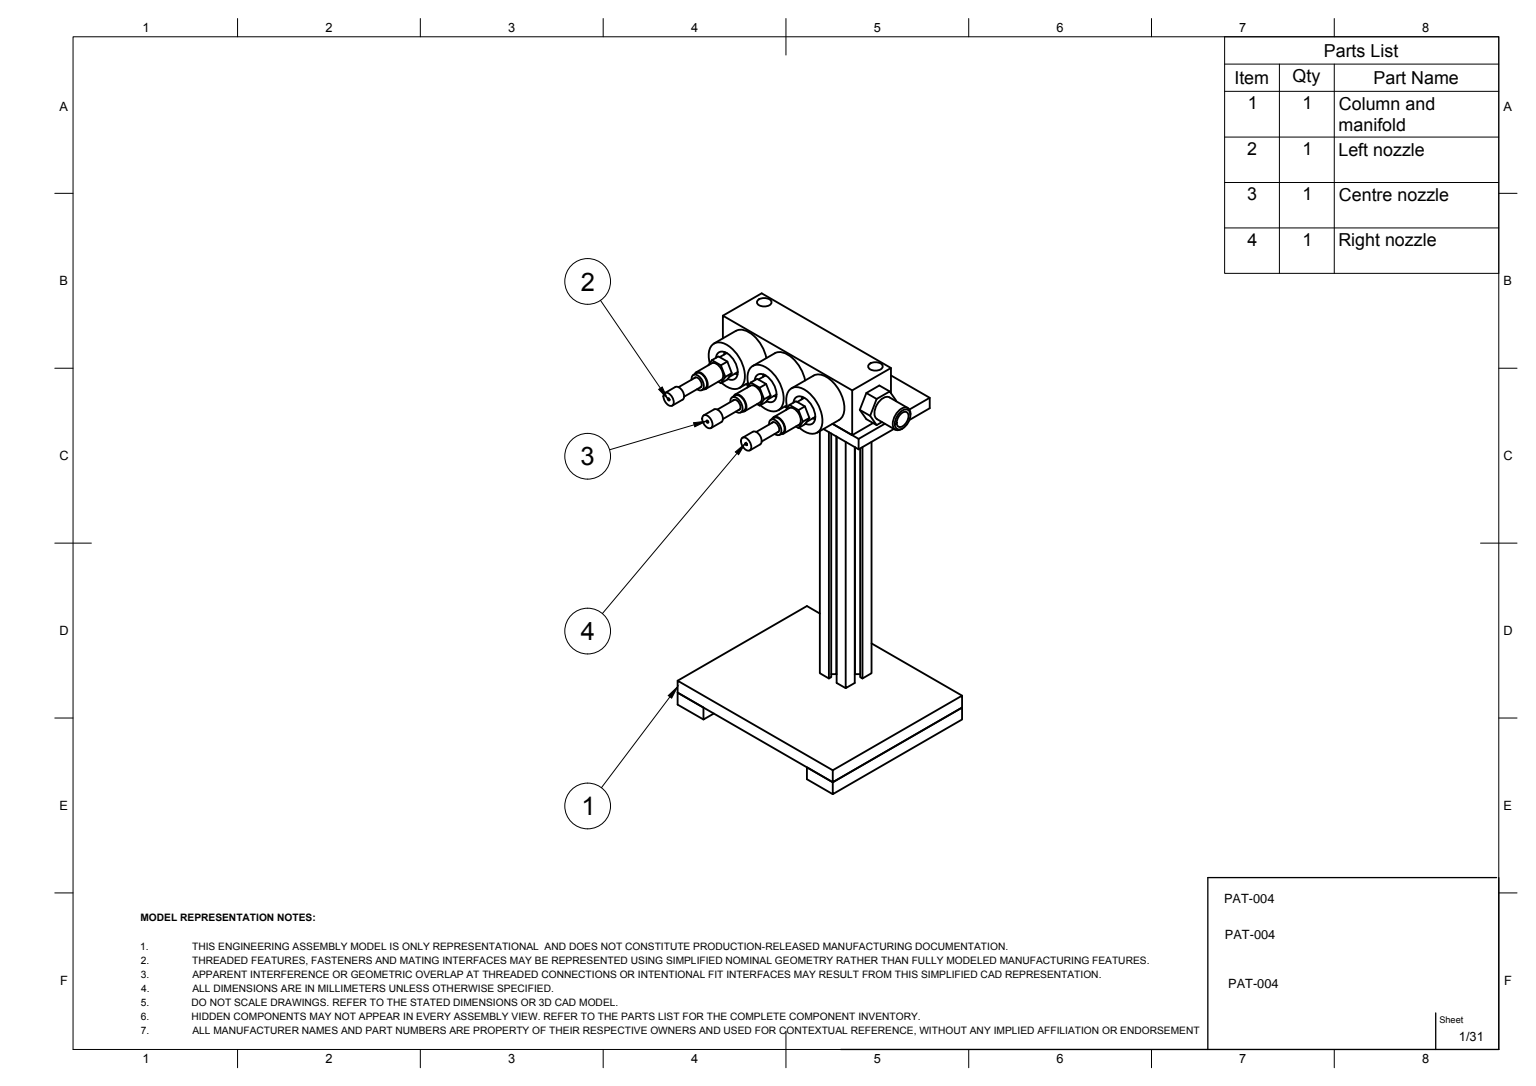
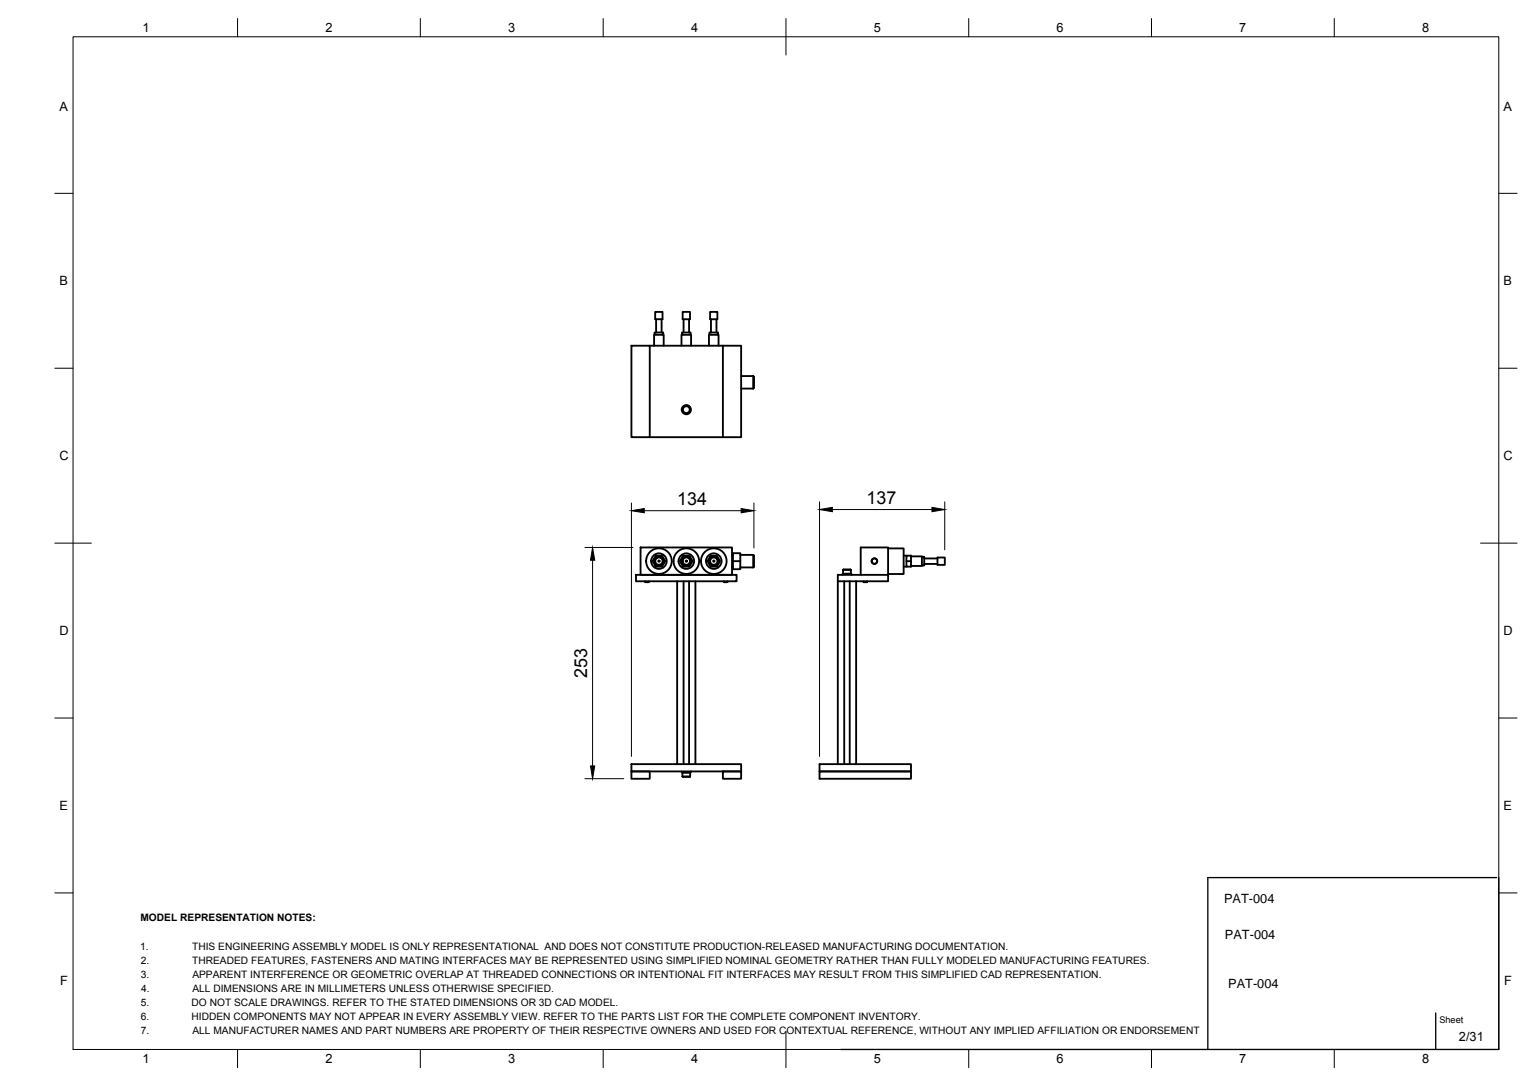
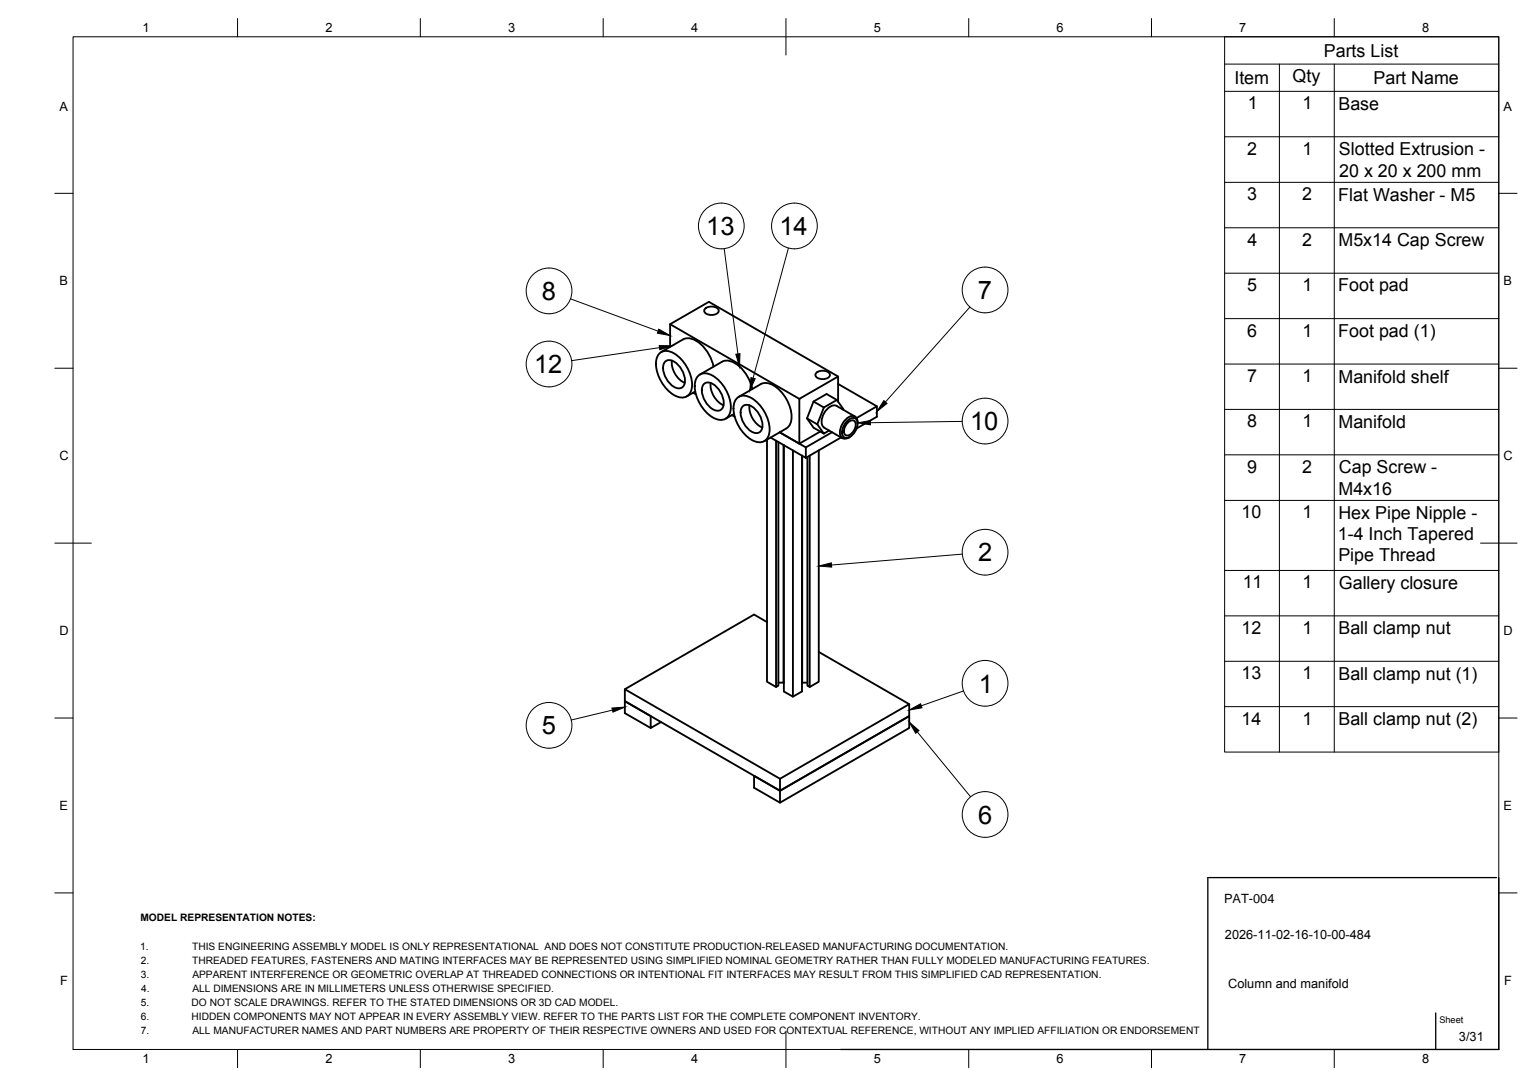
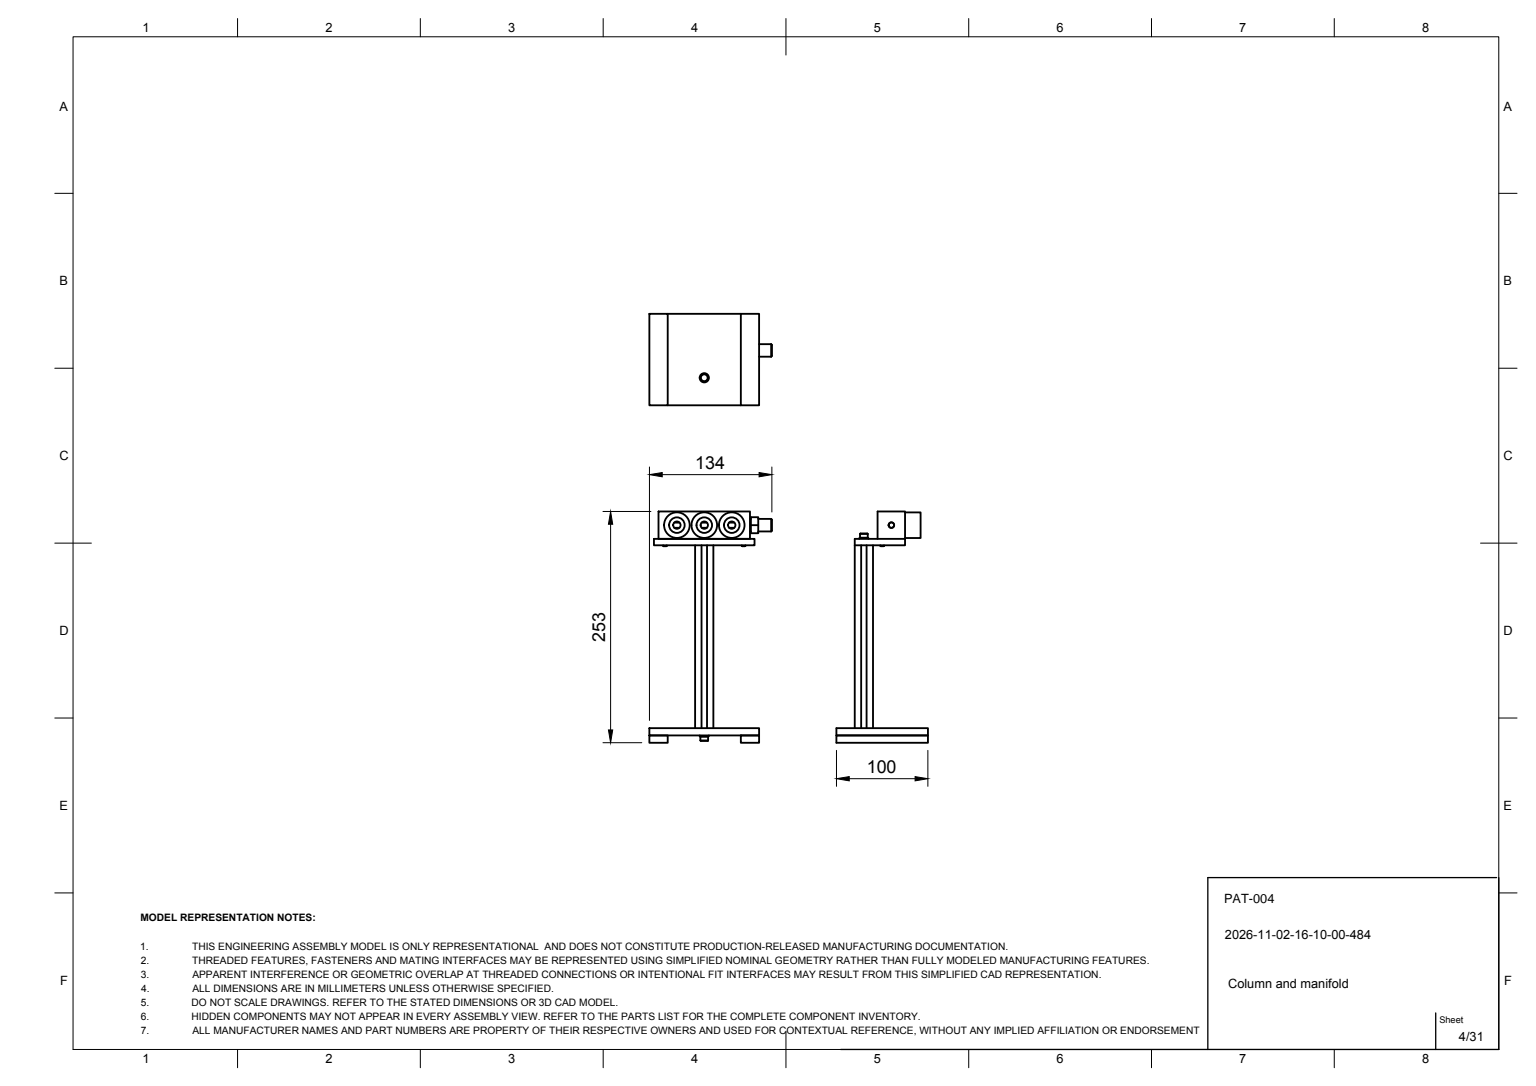
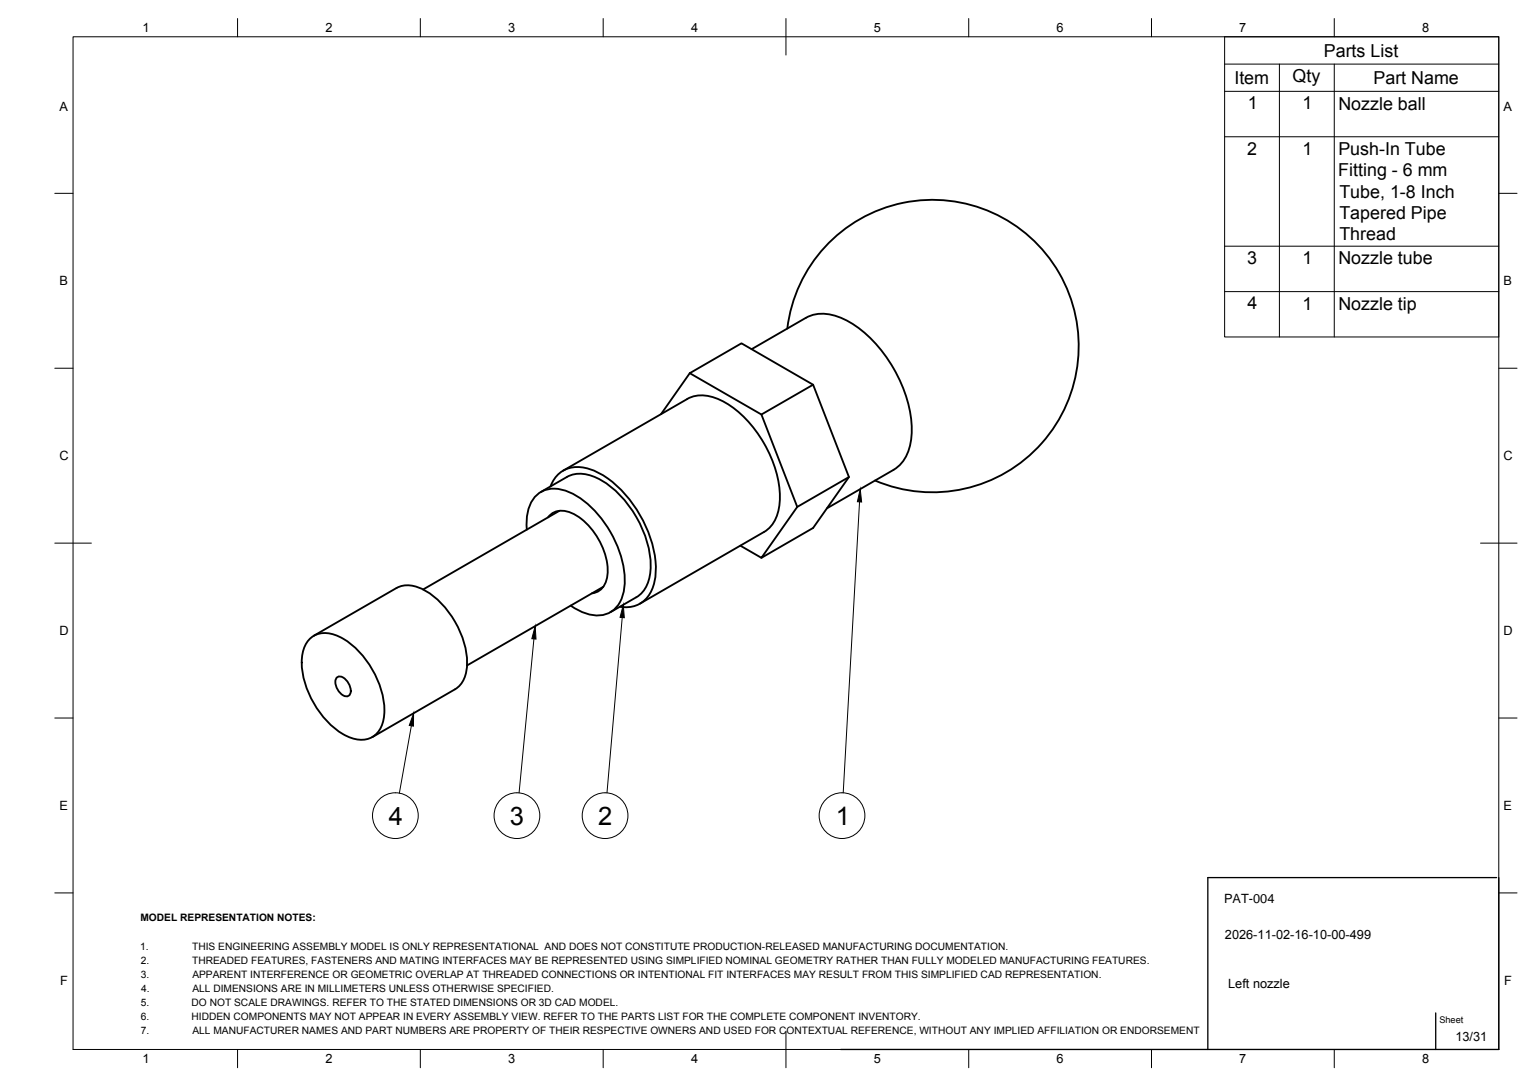
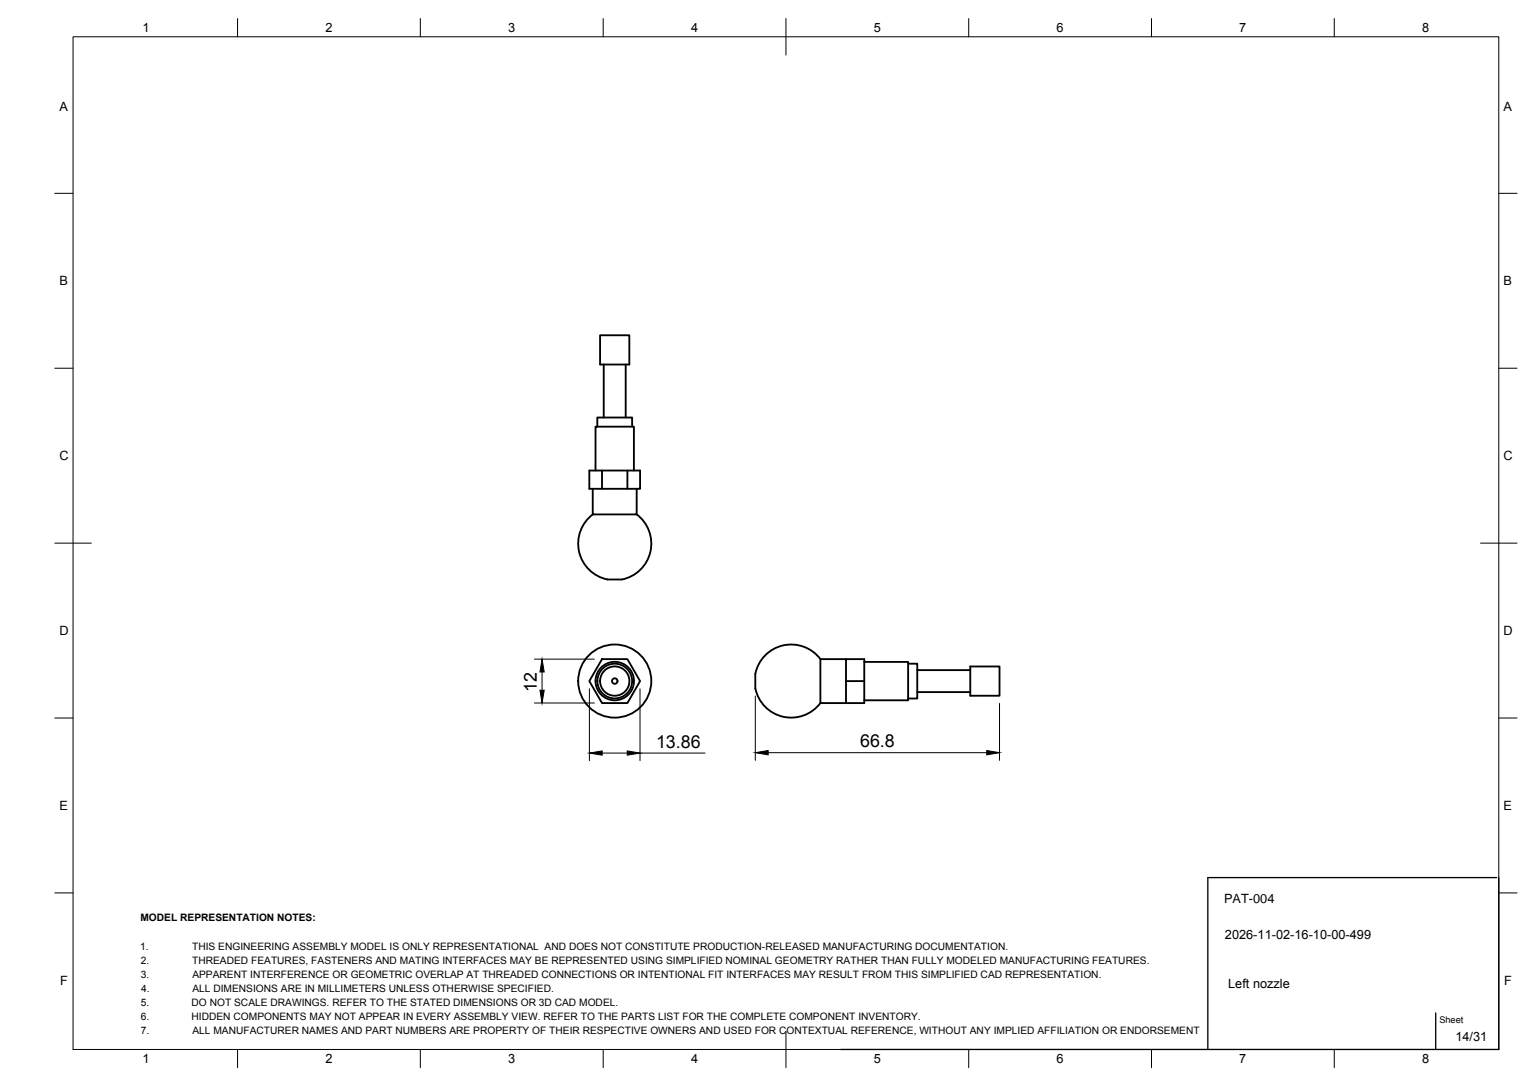
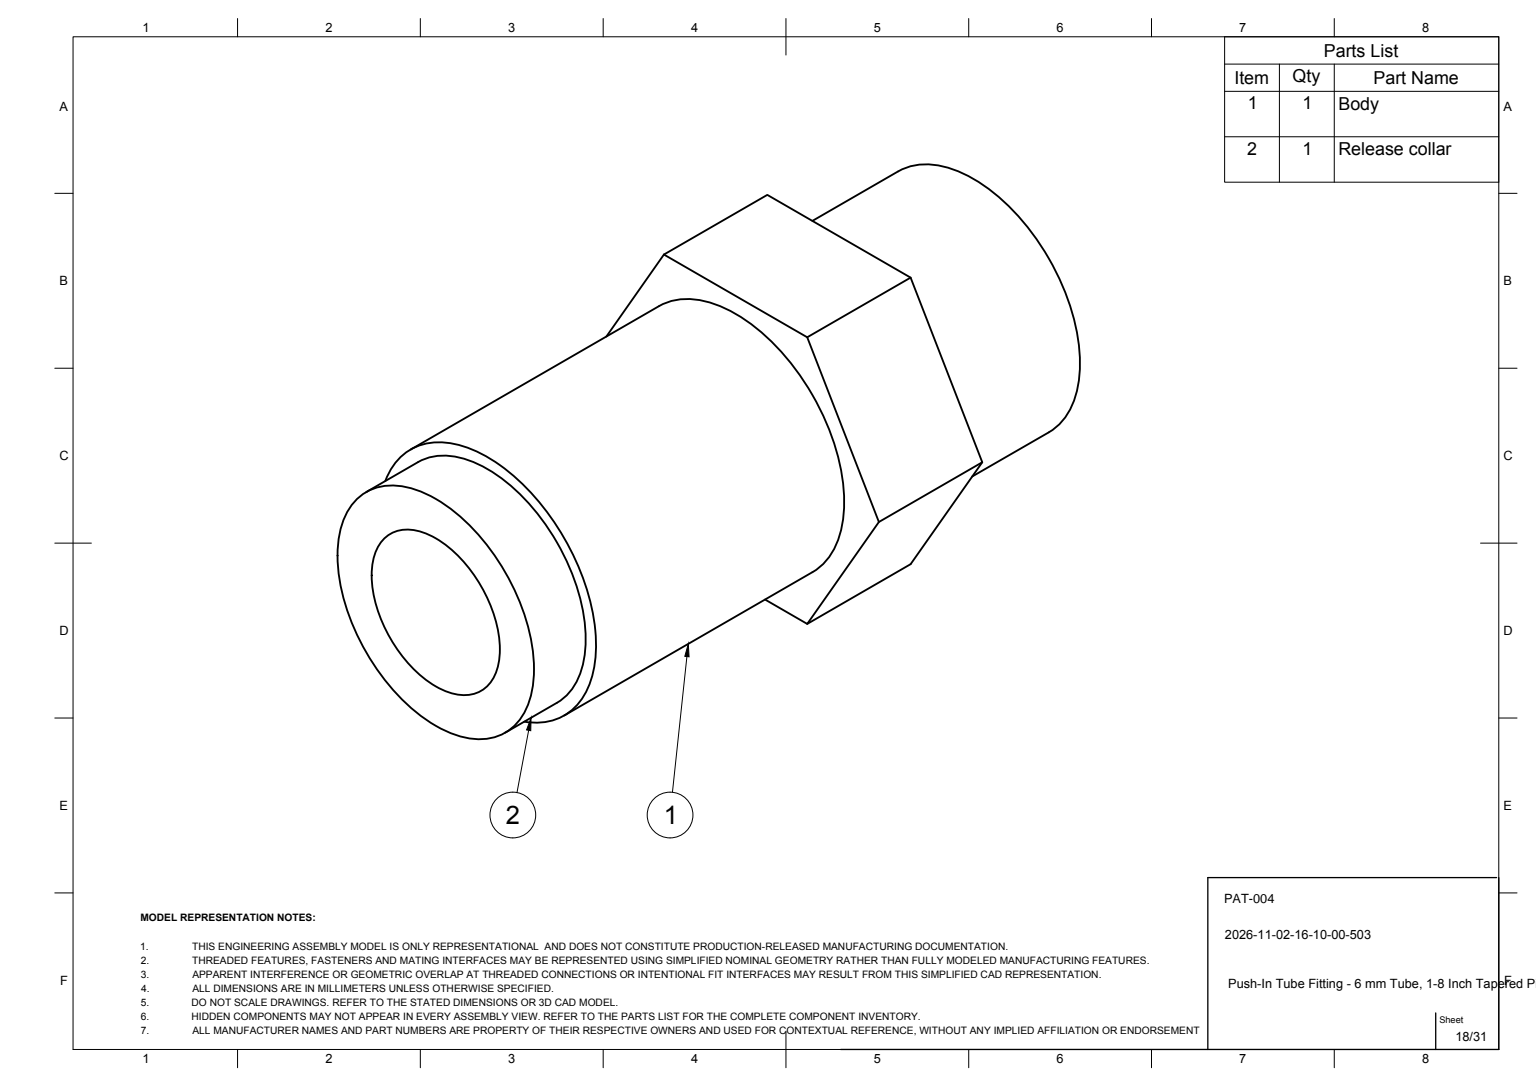
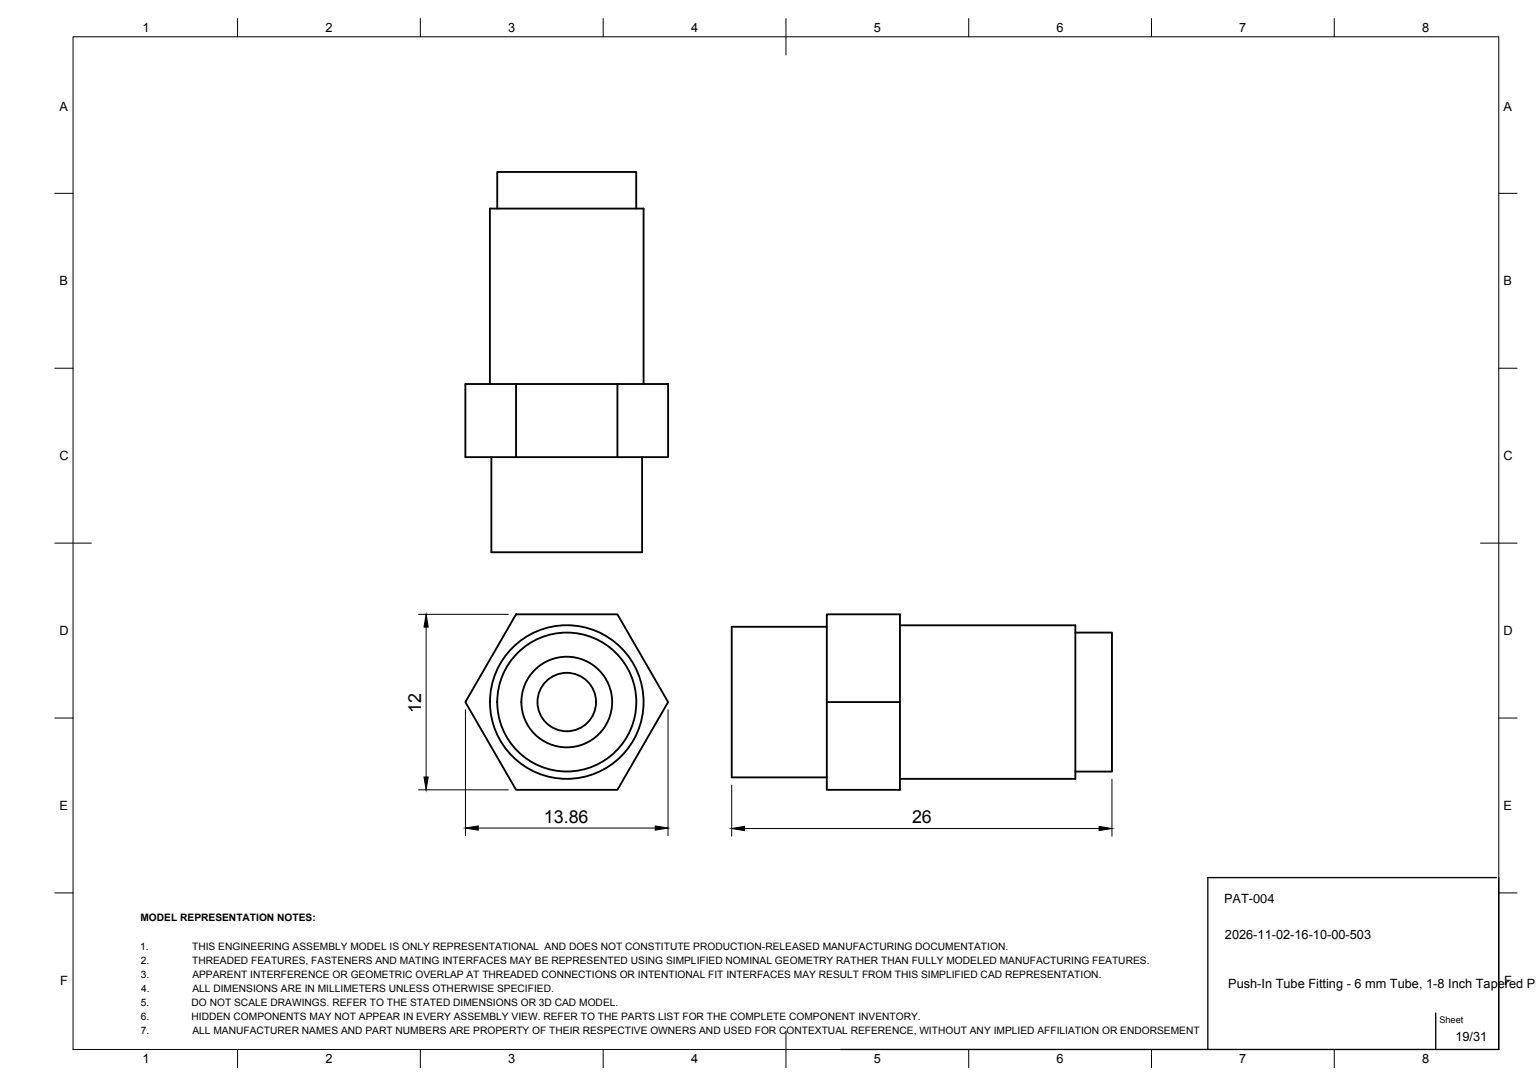
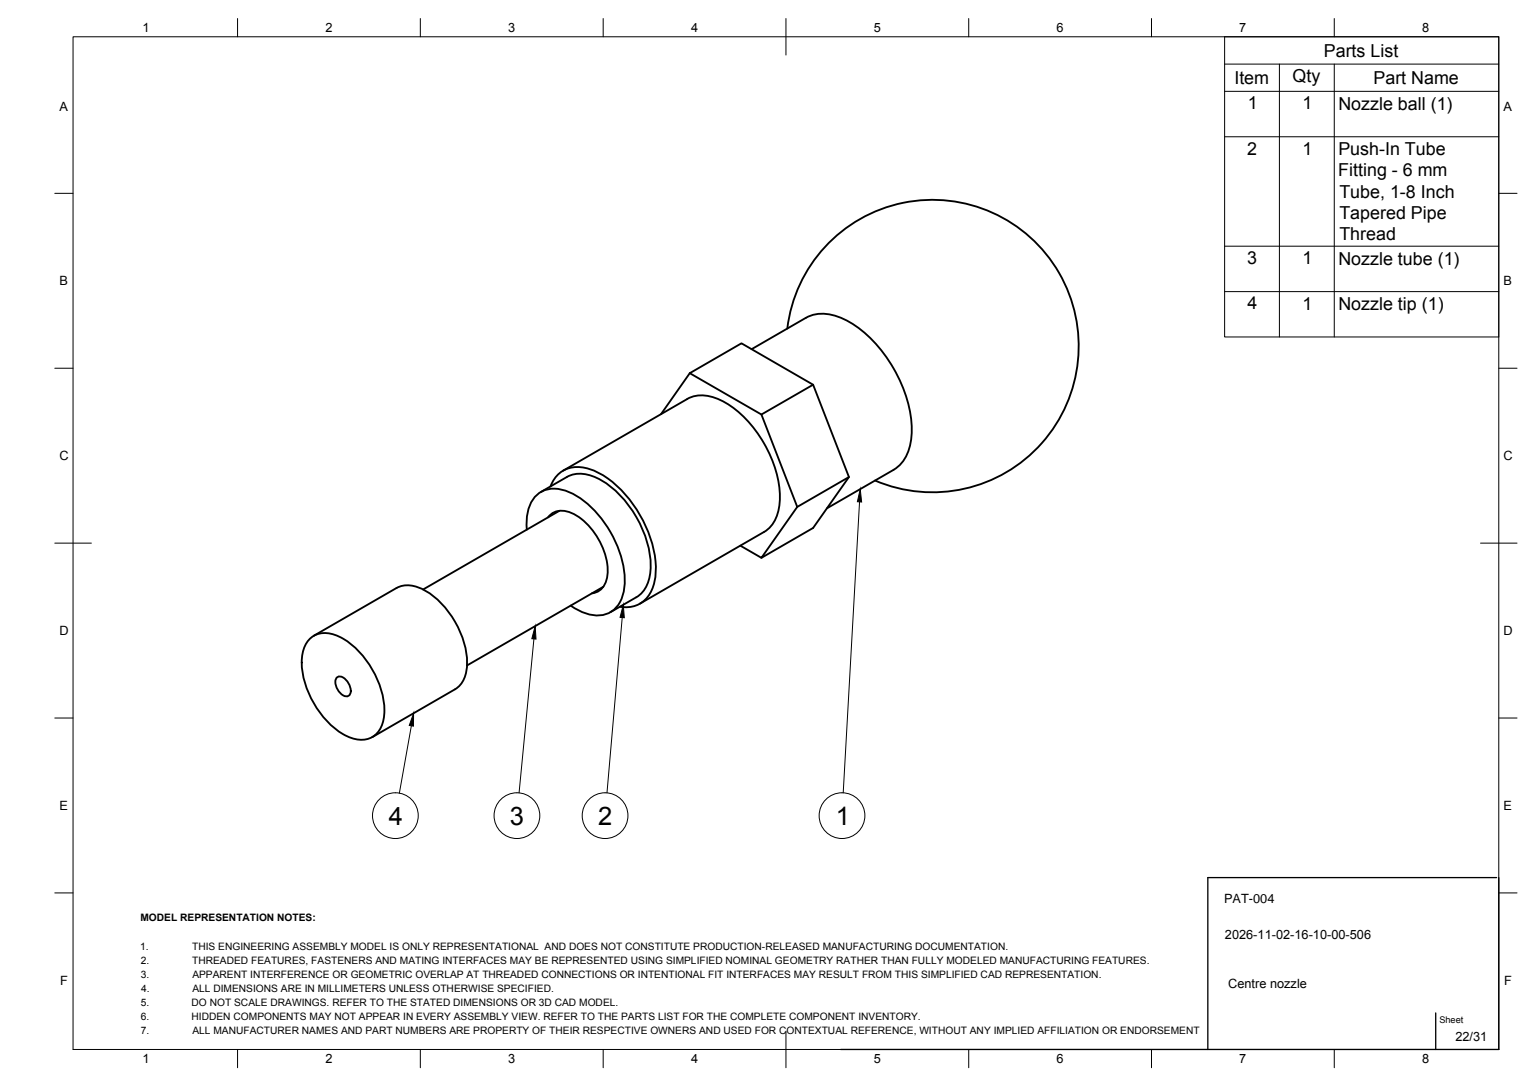
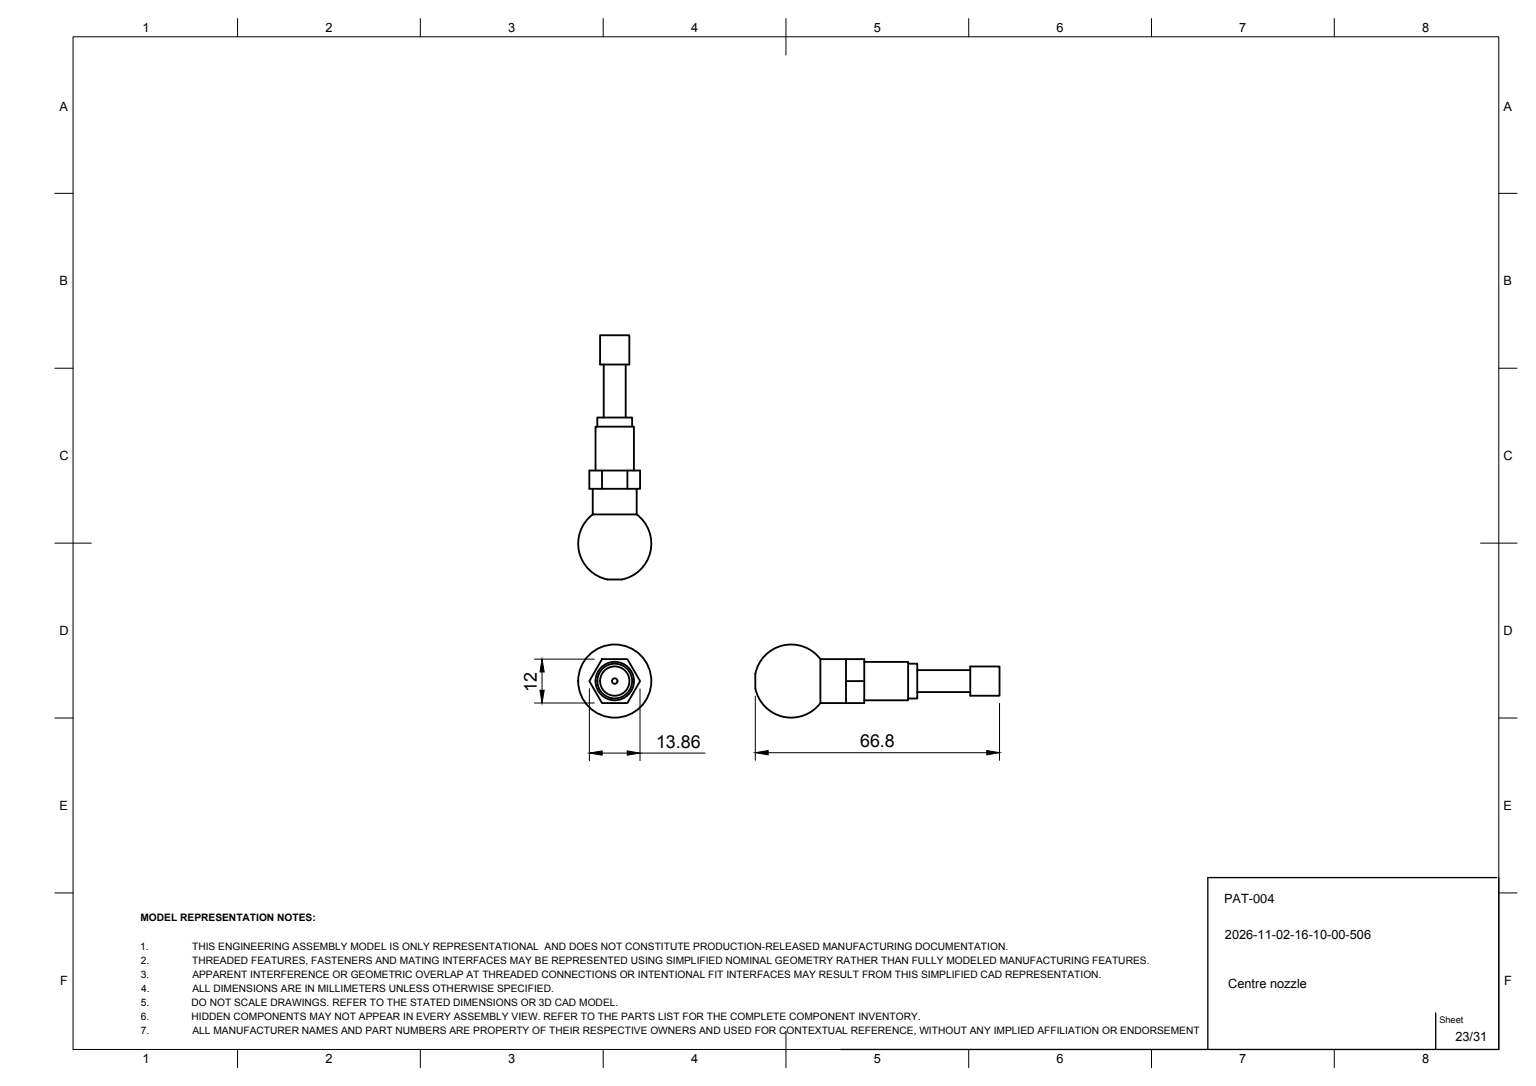
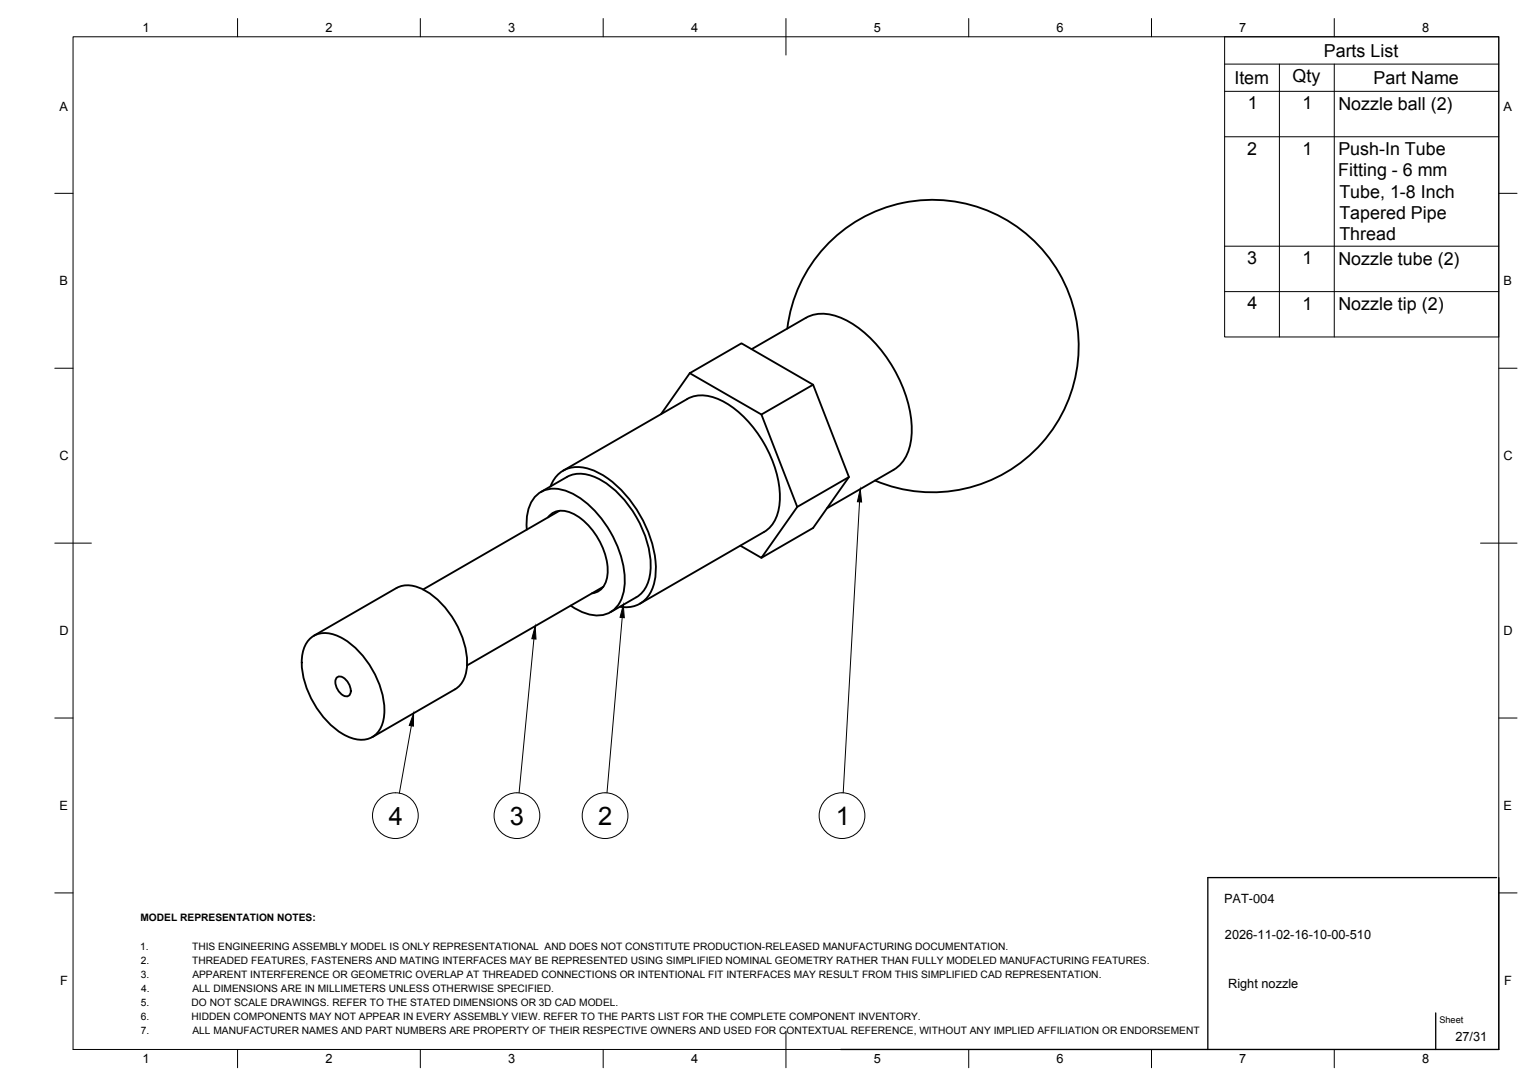
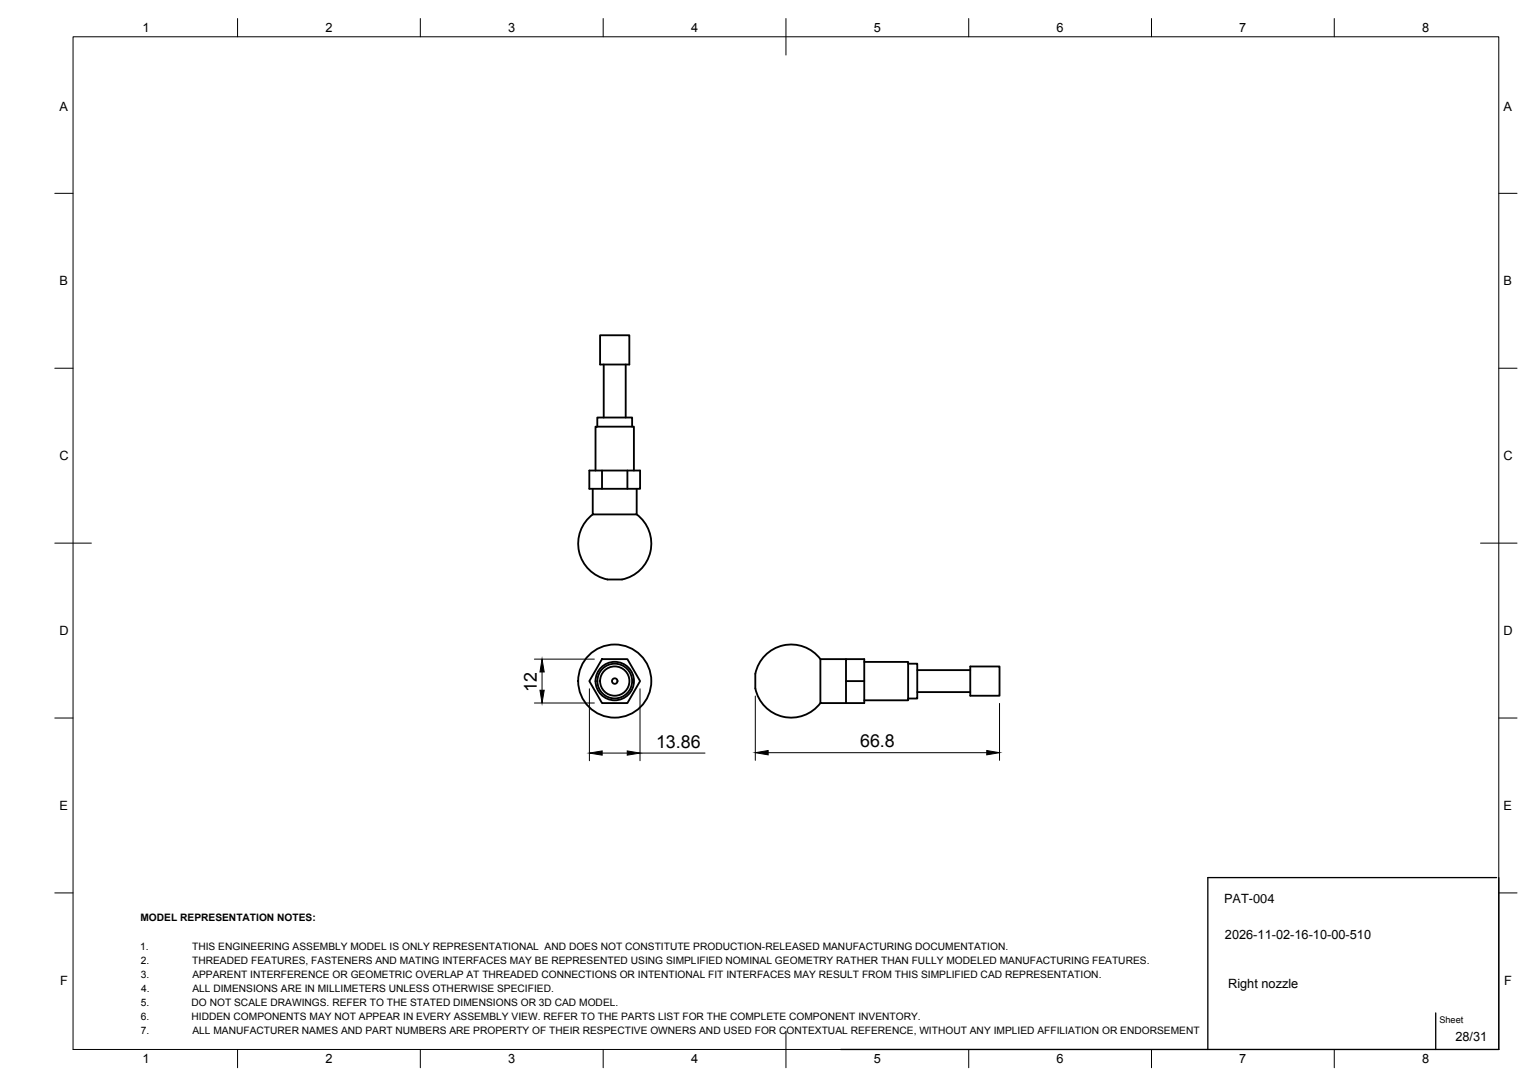
ISO-10303-21;
HEADER;
/* Generated by software containing ST-Developer
 * from STEP Tools, Inc. (www.steptools.com) 
 */

FILE_DESCRIPTION(
/* description */ ('Air blow-off nozzle station'),
/* implementation_level */ '2;1');

FILE_NAME(
/* name */ 'PAT-004',
/* time_stamp */ '2026-10-27T10:53:54-07:00',
/* author */ (''),
/* organization */ (''),
/* preprocessor_version */ 'ST-DEVELOPER v20.2',
/* originating_system */ 'Autodesk Translation Framework v15.17.0.0',
/* authorisation */ '');

FILE_SCHEMA (('AUTOMOTIVE_DESIGN { 1 0 10303 214 3 1 1 }'));
ENDSEC;

DATA;
#10=MECHANICAL_DESIGN_GEOMETRIC_PRESENTATION_REPRESENTATION('',(#237,#238,
#239,#240,#241,#242,#243,#244,#245,#246,#247,#248,#249,#250,#251,#252,#253,
#254,#255,#256,#257,#258,#259,#260,#261),#7897);
#11=ITEM_DEFINED_TRANSFORMATION($,$,#4591,#4884);
#12=ITEM_DEFINED_TRANSFORMATION($,$,#4601,#4885);
#13=ITEM_DEFINED_TRANSFORMATION($,$,#4608,#4886);
#14=ITEM_DEFINED_TRANSFORMATION($,$,#4615,#4887);
#15=ITEM_DEFINED_TRANSFORMATION($,$,#4631,#4888);
#16=ITEM_DEFINED_TRANSFORMATION($,$,#4689,#4889);
#17=ITEM_DEFINED_TRANSFORMATION($,$,#4695,#4890);
#18=ITEM_DEFINED_TRANSFORMATION($,$,#4713,#4891);
#19=ITEM_DEFINED_TRANSFORMATION($,$,#4731,#4892);
#20=ITEM_DEFINED_TRANSFORMATION($,$,#4749,#4893);
#21=ITEM_DEFINED_TRANSFORMATION($,$,#4799,#4894);
#22=ITEM_DEFINED_TRANSFORMATION($,$,#4810,#4895);
#23=ITEM_DEFINED_TRANSFORMATION($,$,#4799,#4896);
#24=ITEM_DEFINED_TRANSFORMATION($,$,#4810,#4897);
#25=ITEM_DEFINED_TRANSFORMATION($,$,#4834,#4898);
#26=ITEM_DEFINED_TRANSFORMATION($,$,#4834,#4899);
#27=ITEM_DEFINED_TRANSFORMATION($,$,#4860,#4900);
#28=ITEM_DEFINED_TRANSFORMATION($,$,#5013,#5054);
#29=ITEM_DEFINED_TRANSFORMATION($,$,#5041,#5055);
#30=ITEM_DEFINED_TRANSFORMATION($,$,#4902,#5056);
#31=ITEM_DEFINED_TRANSFORMATION($,$,#4916,#5057);
#32=ITEM_DEFINED_TRANSFORMATION($,$,#4925,#5058);
#33=ITEM_DEFINED_TRANSFORMATION($,$,#5012,#5059);
#34=ITEM_DEFINED_TRANSFORMATION($,$,#4939,#5060);
#35=ITEM_DEFINED_TRANSFORMATION($,$,#4953,#5061);
#36=ITEM_DEFINED_TRANSFORMATION($,$,#4962,#5062);
#37=ITEM_DEFINED_TRANSFORMATION($,$,#5012,#5063);
#38=ITEM_DEFINED_TRANSFORMATION($,$,#4976,#5064);
#39=ITEM_DEFINED_TRANSFORMATION($,$,#4990,#5065);
#40=ITEM_DEFINED_TRANSFORMATION($,$,#4999,#5066);
#41=ITEM_DEFINED_TRANSFORMATION($,$,#5012,#5067);
#42=ITEM_DEFINED_TRANSFORMATION($,$,#4590,#5068);
#43=ITEM_DEFINED_TRANSFORMATION($,$,#4901,#5069);
#44=ITEM_DEFINED_TRANSFORMATION($,$,#4938,#5070);
#45=ITEM_DEFINED_TRANSFORMATION($,$,#4975,#5071);
#46=(
REPRESENTATION_RELATIONSHIP($,$,#8001,#8000)
REPRESENTATION_RELATIONSHIP_WITH_TRANSFORMATION(#11)
SHAPE_REPRESENTATION_RELATIONSHIP()
);
#47=(
REPRESENTATION_RELATIONSHIP($,$,#8002,#8000)
REPRESENTATION_RELATIONSHIP_WITH_TRANSFORMATION(#12)
SHAPE_REPRESENTATION_RELATIONSHIP()
);
#48=(
REPRESENTATION_RELATIONSHIP($,$,#8003,#8000)
REPRESENTATION_RELATIONSHIP_WITH_TRANSFORMATION(#13)
SHAPE_REPRESENTATION_RELATIONSHIP()
);
#49=(
REPRESENTATION_RELATIONSHIP($,$,#8004,#8000)
REPRESENTATION_RELATIONSHIP_WITH_TRANSFORMATION(#14)
SHAPE_REPRESENTATION_RELATIONSHIP()
);
#50=(
REPRESENTATION_RELATIONSHIP($,$,#8005,#8000)
REPRESENTATION_RELATIONSHIP_WITH_TRANSFORMATION(#15)
SHAPE_REPRESENTATION_RELATIONSHIP()
);
#51=(
REPRESENTATION_RELATIONSHIP($,$,#8006,#8000)
REPRESENTATION_RELATIONSHIP_WITH_TRANSFORMATION(#16)
SHAPE_REPRESENTATION_RELATIONSHIP()
);
#52=(
REPRESENTATION_RELATIONSHIP($,$,#8007,#8000)
REPRESENTATION_RELATIONSHIP_WITH_TRANSFORMATION(#17)
SHAPE_REPRESENTATION_RELATIONSHIP()
);
#53=(
REPRESENTATION_RELATIONSHIP($,$,#8008,#8000)
REPRESENTATION_RELATIONSHIP_WITH_TRANSFORMATION(#18)
SHAPE_REPRESENTATION_RELATIONSHIP()
);
#54=(
REPRESENTATION_RELATIONSHIP($,$,#8009,#8000)
REPRESENTATION_RELATIONSHIP_WITH_TRANSFORMATION(#19)
SHAPE_REPRESENTATION_RELATIONSHIP()
);
#55=(
REPRESENTATION_RELATIONSHIP($,$,#8010,#8000)
REPRESENTATION_RELATIONSHIP_WITH_TRANSFORMATION(#20)
SHAPE_REPRESENTATION_RELATIONSHIP()
);
#56=(
REPRESENTATION_RELATIONSHIP($,$,#8011,#8000)
REPRESENTATION_RELATIONSHIP_WITH_TRANSFORMATION(#21)
SHAPE_REPRESENTATION_RELATIONSHIP()
);
#57=(
REPRESENTATION_RELATIONSHIP($,$,#8012,#8000)
REPRESENTATION_RELATIONSHIP_WITH_TRANSFORMATION(#22)
SHAPE_REPRESENTATION_RELATIONSHIP()
);
#58=(
REPRESENTATION_RELATIONSHIP($,$,#8011,#8000)
REPRESENTATION_RELATIONSHIP_WITH_TRANSFORMATION(#23)
SHAPE_REPRESENTATION_RELATIONSHIP()
);
#59=(
REPRESENTATION_RELATIONSHIP($,$,#8012,#8000)
REPRESENTATION_RELATIONSHIP_WITH_TRANSFORMATION(#24)
SHAPE_REPRESENTATION_RELATIONSHIP()
);
#60=(
REPRESENTATION_RELATIONSHIP($,$,#8013,#8000)
REPRESENTATION_RELATIONSHIP_WITH_TRANSFORMATION(#25)
SHAPE_REPRESENTATION_RELATIONSHIP()
);
#61=(
REPRESENTATION_RELATIONSHIP($,$,#8013,#8000)
REPRESENTATION_RELATIONSHIP_WITH_TRANSFORMATION(#26)
SHAPE_REPRESENTATION_RELATIONSHIP()
);
#62=(
REPRESENTATION_RELATIONSHIP($,$,#8014,#8000)
REPRESENTATION_RELATIONSHIP_WITH_TRANSFORMATION(#27)
SHAPE_REPRESENTATION_RELATIONSHIP()
);
#63=(
REPRESENTATION_RELATIONSHIP($,$,#8028,#8027)
REPRESENTATION_RELATIONSHIP_WITH_TRANSFORMATION(#28)
SHAPE_REPRESENTATION_RELATIONSHIP()
);
#64=(
REPRESENTATION_RELATIONSHIP($,$,#8029,#8027)
REPRESENTATION_RELATIONSHIP_WITH_TRANSFORMATION(#29)
SHAPE_REPRESENTATION_RELATIONSHIP()
);
#65=(
REPRESENTATION_RELATIONSHIP($,$,#8016,#8015)
REPRESENTATION_RELATIONSHIP_WITH_TRANSFORMATION(#30)
SHAPE_REPRESENTATION_RELATIONSHIP()
);
#66=(
REPRESENTATION_RELATIONSHIP($,$,#8017,#8015)
REPRESENTATION_RELATIONSHIP_WITH_TRANSFORMATION(#31)
SHAPE_REPRESENTATION_RELATIONSHIP()
);
#67=(
REPRESENTATION_RELATIONSHIP($,$,#8018,#8015)
REPRESENTATION_RELATIONSHIP_WITH_TRANSFORMATION(#32)
SHAPE_REPRESENTATION_RELATIONSHIP()
);
#68=(
REPRESENTATION_RELATIONSHIP($,$,#8027,#8015)
REPRESENTATION_RELATIONSHIP_WITH_TRANSFORMATION(#33)
SHAPE_REPRESENTATION_RELATIONSHIP()
);
#69=(
REPRESENTATION_RELATIONSHIP($,$,#8020,#8019)
REPRESENTATION_RELATIONSHIP_WITH_TRANSFORMATION(#34)
SHAPE_REPRESENTATION_RELATIONSHIP()
);
#70=(
REPRESENTATION_RELATIONSHIP($,$,#8021,#8019)
REPRESENTATION_RELATIONSHIP_WITH_TRANSFORMATION(#35)
SHAPE_REPRESENTATION_RELATIONSHIP()
);
#71=(
REPRESENTATION_RELATIONSHIP($,$,#8022,#8019)
REPRESENTATION_RELATIONSHIP_WITH_TRANSFORMATION(#36)
SHAPE_REPRESENTATION_RELATIONSHIP()
);
#72=(
REPRESENTATION_RELATIONSHIP($,$,#8027,#8019)
REPRESENTATION_RELATIONSHIP_WITH_TRANSFORMATION(#37)
SHAPE_REPRESENTATION_RELATIONSHIP()
);
#73=(
REPRESENTATION_RELATIONSHIP($,$,#8024,#8023)
REPRESENTATION_RELATIONSHIP_WITH_TRANSFORMATION(#38)
SHAPE_REPRESENTATION_RELATIONSHIP()
);
#74=(
REPRESENTATION_RELATIONSHIP($,$,#8025,#8023)
REPRESENTATION_RELATIONSHIP_WITH_TRANSFORMATION(#39)
SHAPE_REPRESENTATION_RELATIONSHIP()
);
#75=(
REPRESENTATION_RELATIONSHIP($,$,#8026,#8023)
REPRESENTATION_RELATIONSHIP_WITH_TRANSFORMATION(#40)
SHAPE_REPRESENTATION_RELATIONSHIP()
);
#76=(
REPRESENTATION_RELATIONSHIP($,$,#8027,#8023)
REPRESENTATION_RELATIONSHIP_WITH_TRANSFORMATION(#41)
SHAPE_REPRESENTATION_RELATIONSHIP()
);
#77=(
REPRESENTATION_RELATIONSHIP($,$,#8000,#7999)
REPRESENTATION_RELATIONSHIP_WITH_TRANSFORMATION(#42)
SHAPE_REPRESENTATION_RELATIONSHIP()
);
#78=(
REPRESENTATION_RELATIONSHIP($,$,#8015,#7999)
REPRESENTATION_RELATIONSHIP_WITH_TRANSFORMATION(#43)
SHAPE_REPRESENTATION_RELATIONSHIP()
);
#79=(
REPRESENTATION_RELATIONSHIP($,$,#8019,#7999)
REPRESENTATION_RELATIONSHIP_WITH_TRANSFORMATION(#44)
SHAPE_REPRESENTATION_RELATIONSHIP()
);
#80=(
REPRESENTATION_RELATIONSHIP($,$,#8023,#7999)
REPRESENTATION_RELATIONSHIP_WITH_TRANSFORMATION(#45)
SHAPE_REPRESENTATION_RELATIONSHIP()
);
#81=CONTEXT_DEPENDENT_SHAPE_REPRESENTATION(#46,#7949);
#82=CONTEXT_DEPENDENT_SHAPE_REPRESENTATION(#47,#7950);
#83=CONTEXT_DEPENDENT_SHAPE_REPRESENTATION(#48,#7951);
#84=CONTEXT_DEPENDENT_SHAPE_REPRESENTATION(#49,#7952);
#85=CONTEXT_DEPENDENT_SHAPE_REPRESENTATION(#50,#7953);
#86=CONTEXT_DEPENDENT_SHAPE_REPRESENTATION(#51,#7954);
#87=CONTEXT_DEPENDENT_SHAPE_REPRESENTATION(#52,#7955);
#88=CONTEXT_DEPENDENT_SHAPE_REPRESENTATION(#53,#7956);
#89=CONTEXT_DEPENDENT_SHAPE_REPRESENTATION(#54,#7957);
#90=CONTEXT_DEPENDENT_SHAPE_REPRESENTATION(#55,#7958);
#91=CONTEXT_DEPENDENT_SHAPE_REPRESENTATION(#56,#7959);
#92=CONTEXT_DEPENDENT_SHAPE_REPRESENTATION(#57,#7960);
#93=CONTEXT_DEPENDENT_SHAPE_REPRESENTATION(#58,#7961);
#94=CONTEXT_DEPENDENT_SHAPE_REPRESENTATION(#59,#7962);
#95=CONTEXT_DEPENDENT_SHAPE_REPRESENTATION(#60,#7963);
#96=CONTEXT_DEPENDENT_SHAPE_REPRESENTATION(#61,#7964);
#97=CONTEXT_DEPENDENT_SHAPE_REPRESENTATION(#62,#7965);
#98=CONTEXT_DEPENDENT_SHAPE_REPRESENTATION(#63,#7981);
#99=CONTEXT_DEPENDENT_SHAPE_REPRESENTATION(#64,#7982);
#100=CONTEXT_DEPENDENT_SHAPE_REPRESENTATION(#65,#7983);
#101=CONTEXT_DEPENDENT_SHAPE_REPRESENTATION(#66,#7984);
#102=CONTEXT_DEPENDENT_SHAPE_REPRESENTATION(#67,#7985);
#103=CONTEXT_DEPENDENT_SHAPE_REPRESENTATION(#68,#7986);
#104=CONTEXT_DEPENDENT_SHAPE_REPRESENTATION(#69,#7987);
#105=CONTEXT_DEPENDENT_SHAPE_REPRESENTATION(#70,#7988);
#106=CONTEXT_DEPENDENT_SHAPE_REPRESENTATION(#71,#7989);
#107=CONTEXT_DEPENDENT_SHAPE_REPRESENTATION(#72,#7990);
#108=CONTEXT_DEPENDENT_SHAPE_REPRESENTATION(#73,#7991);
#109=CONTEXT_DEPENDENT_SHAPE_REPRESENTATION(#74,#7992);
#110=CONTEXT_DEPENDENT_SHAPE_REPRESENTATION(#75,#7993);
#111=CONTEXT_DEPENDENT_SHAPE_REPRESENTATION(#76,#7994);
#112=CONTEXT_DEPENDENT_SHAPE_REPRESENTATION(#77,#7995);
#113=CONTEXT_DEPENDENT_SHAPE_REPRESENTATION(#78,#7996);
#114=CONTEXT_DEPENDENT_SHAPE_REPRESENTATION(#79,#7997);
#115=CONTEXT_DEPENDENT_SHAPE_REPRESENTATION(#80,#7998);
#116=NEXT_ASSEMBLY_USAGE_OCCURRENCE('Base:1','Base:1','Base:1',#8032,#8033,
'Base:1');
#117=NEXT_ASSEMBLY_USAGE_OCCURRENCE('Foot pad:1','Foot pad:1',
'Foot pad:1',#8032,#8034,'Foot pad:1');
#118=NEXT_ASSEMBLY_USAGE_OCCURRENCE('Foot pad (1):1','Foot pad (1):1',
'Foot pad (1):1',#8032,#8035,'Foot pad (1):1');
#119=NEXT_ASSEMBLY_USAGE_OCCURRENCE('Manifold shelf:1',
'Manifold shelf:1','Manifold shelf:1',#8032,#8036,'Manifold shelf:1');
#120=NEXT_ASSEMBLY_USAGE_OCCURRENCE('Manifold:1','Manifold:1',
'Manifold:1',#8032,#8037,'Manifold:1');
#121=NEXT_ASSEMBLY_USAGE_OCCURRENCE('Gallery closure:1',
'Gallery closure:1','Gallery closure:1',#8032,#8038,'Gallery closure:1');
#122=NEXT_ASSEMBLY_USAGE_OCCURRENCE('Ball clamp nut:1',
'Ball clamp nut:1','Ball clamp nut:1',#8032,#8039,'Ball clamp nut:1');
#123=NEXT_ASSEMBLY_USAGE_OCCURRENCE('Ball clamp nut (1):1',
'Ball clamp nut (1):1','Ball clamp nut (1):1',#8032,#8040,
'Ball clamp nut (1):1');
#124=NEXT_ASSEMBLY_USAGE_OCCURRENCE('Ball clamp nut (2):1',
'Ball clamp nut (2):1','Ball clamp nut (2):1',#8032,#8041,
'Ball clamp nut (2):1');
#125=NEXT_ASSEMBLY_USAGE_OCCURRENCE(
'Slotted Extrusion - 20 x 20 x 200 mm:2',
'Slotted Extrusion - 20 x 20 x 200 mm:2',
'Slotted Extrusion - 20 x 20 x 200 mm:2',#8032,#8042,
'Slotted Extrusion - 20 x 20 x 200 mm:2');
#126=NEXT_ASSEMBLY_USAGE_OCCURRENCE('Flat Washer - M5:2',
'Flat Washer - M5:2','Flat Washer - M5:2',#8032,#8043,
'Flat Washer - M5:2');
#127=NEXT_ASSEMBLY_USAGE_OCCURRENCE('M5x14 Cap Screw:2',
'M5x14 Cap Screw:2','M5x14 Cap Screw:2',#8032,#8044,'M5x14 Cap Screw:2');
#128=NEXT_ASSEMBLY_USAGE_OCCURRENCE('Flat Washer - M5:3',
'Flat Washer - M5:3','Flat Washer - M5:3',#8032,#8043,
'Flat Washer - M5:3');
#129=NEXT_ASSEMBLY_USAGE_OCCURRENCE('M5x14 Cap Screw:3',
'M5x14 Cap Screw:3','M5x14 Cap Screw:3',#8032,#8044,'M5x14 Cap Screw:3');
#130=NEXT_ASSEMBLY_USAGE_OCCURRENCE('Cap Screw - M4x16:2',
'Cap Screw - M4x16:2','Cap Screw - M4x16:2',#8032,#8045,
'Cap Screw - M4x16:2');
#131=NEXT_ASSEMBLY_USAGE_OCCURRENCE('Cap Screw - M4x16:3',
'Cap Screw - M4x16:3','Cap Screw - M4x16:3',#8032,#8045,
'Cap Screw - M4x16:3');
#132=NEXT_ASSEMBLY_USAGE_OCCURRENCE(
'Hex Pipe Nipple - 1-4 Inch Tapered Pipe Thread:2',
'Hex Pipe Nipple - 1-4 Inch Tapered Pipe Thread:2',
'Hex Pipe Nipple - 1-4 Inch Tapered Pipe Thread:2',#8032,#8046,
'Hex Pipe Nipple - 1-4 Inch Tapered Pipe Thread:2');
#133=NEXT_ASSEMBLY_USAGE_OCCURRENCE('Body:1','Body:1','Body:1',#8059,#8060,
'Body:1');
#134=NEXT_ASSEMBLY_USAGE_OCCURRENCE('Release collar:1',
'Release collar:1','Release collar:1',#8059,#8061,'Release collar:1');
#135=NEXT_ASSEMBLY_USAGE_OCCURRENCE('Nozzle ball:1','Nozzle ball:1',
'Nozzle ball:1',#8047,#8048,'Nozzle ball:1');
#136=NEXT_ASSEMBLY_USAGE_OCCURRENCE('Nozzle tube:1','Nozzle tube:1',
'Nozzle tube:1',#8047,#8049,'Nozzle tube:1');
#137=NEXT_ASSEMBLY_USAGE_OCCURRENCE('Nozzle tip:1','Nozzle tip:1',
'Nozzle tip:1',#8047,#8050,'Nozzle tip:1');
#138=NEXT_ASSEMBLY_USAGE_OCCURRENCE(
'Push-In Tube Fitting - 6 mm Tube, 1-8 Inch Tapered Pipe Thread:2',
'Push-In Tube Fitting - 6 mm Tube, 1-8 Inch Tapered Pipe Thread:2',
'Push-In Tube Fitting - 6 mm Tube, 1-8 Inch Tapered Pipe Thread:2',#8047,
#8059,
'Push-In Tube Fitting - 6 mm Tube, 1-8 Inch Tapered Pipe Thread:2');
#139=NEXT_ASSEMBLY_USAGE_OCCURRENCE('Nozzle ball (1):1',
'Nozzle ball (1):1','Nozzle ball (1):1',#8051,#8052,'Nozzle ball (1):1');
#140=NEXT_ASSEMBLY_USAGE_OCCURRENCE('Nozzle tube (1):1',
'Nozzle tube (1):1','Nozzle tube (1):1',#8051,#8053,'Nozzle tube (1):1');
#141=NEXT_ASSEMBLY_USAGE_OCCURRENCE('Nozzle tip (1):1',
'Nozzle tip (1):1','Nozzle tip (1):1',#8051,#8054,'Nozzle tip (1):1');
#142=NEXT_ASSEMBLY_USAGE_OCCURRENCE(
'Push-In Tube Fitting - 6 mm Tube, 1-8 Inch Tapered Pipe Thread:3',
'Push-In Tube Fitting - 6 mm Tube, 1-8 Inch Tapered Pipe Thread:3',
'Push-In Tube Fitting - 6 mm Tube, 1-8 Inch Tapered Pipe Thread:3',#8051,
#8059,
'Push-In Tube Fitting - 6 mm Tube, 1-8 Inch Tapered Pipe Thread:3');
#143=NEXT_ASSEMBLY_USAGE_OCCURRENCE('Nozzle ball (2):1',
'Nozzle ball (2):1','Nozzle ball (2):1',#8055,#8056,'Nozzle ball (2):1');
#144=NEXT_ASSEMBLY_USAGE_OCCURRENCE('Nozzle tube (2):1',
'Nozzle tube (2):1','Nozzle tube (2):1',#8055,#8057,'Nozzle tube (2):1');
#145=NEXT_ASSEMBLY_USAGE_OCCURRENCE('Nozzle tip (2):1',
'Nozzle tip (2):1','Nozzle tip (2):1',#8055,#8058,'Nozzle tip (2):1');
#146=NEXT_ASSEMBLY_USAGE_OCCURRENCE(
'Push-In Tube Fitting - 6 mm Tube, 1-8 Inch Tapered Pipe Thread:4',
'Push-In Tube Fitting - 6 mm Tube, 1-8 Inch Tapered Pipe Thread:4',
'Push-In Tube Fitting - 6 mm Tube, 1-8 Inch Tapered Pipe Thread:4',#8055,
#8059,
'Push-In Tube Fitting - 6 mm Tube, 1-8 Inch Tapered Pipe Thread:4');
#147=NEXT_ASSEMBLY_USAGE_OCCURRENCE('Column and manifold:1',
'Column and manifold:1','Column and manifold:1',#8031,#8032,
'Column and manifold:1');
#148=NEXT_ASSEMBLY_USAGE_OCCURRENCE('Left nozzle:1','Left nozzle:1',
'Left nozzle:1',#8031,#8047,'Left nozzle:1');
#149=NEXT_ASSEMBLY_USAGE_OCCURRENCE('Centre nozzle:1','Centre nozzle:1',
'Centre nozzle:1',#8031,#8051,'Centre nozzle:1');
#150=NEXT_ASSEMBLY_USAGE_OCCURRENCE('Right nozzle:1','Right nozzle:1',
'Right nozzle:1',#8031,#8055,'Right nozzle:1');
#151=ORIENTED_CLOSED_SHELL('',*,#4297,.F.);
#152=ORIENTED_CLOSED_SHELL('',*,#4300,.F.);
#153=BREP_WITH_VOIDS('Body1',#4298,(#151));
#154=BREP_WITH_VOIDS('Body1',#4299,(#152));
#155=CONICAL_SURFACE('',#4800,0.275,0.785398163397449);
#156=CONICAL_SURFACE('',#4823,0.4,0.785398163397448);
#157=CONICAL_SURFACE('',#4827,0.41,0.785398163397448);
#158=CONICAL_SURFACE('',#4831,0.26,0.463647609000806);
#159=CONICAL_SURFACE('',#4837,0.325,0.785398163397448);
#160=CONICAL_SURFACE('',#4841,0.335,0.785398163397448);
#161=CONICAL_SURFACE('',#4845,0.21,0.463647609000806);
#162=CONICAL_SURFACE('',#4849,0.18,0.785398163397448);
#163=CONICAL_SURFACE('',#4876,0.645,0.785398163397448);
#164=CONICAL_SURFACE('',#4879,0.645,0.785398163397448);
#165=SPHERICAL_SURFACE('',#4702,1.);
#166=SPHERICAL_SURFACE('',#4720,1.);
#167=SPHERICAL_SURFACE('',#4738,1.);
#168=SPHERICAL_SURFACE('',#4914,1.);
#169=SPHERICAL_SURFACE('',#4951,1.);
#170=SPHERICAL_SURFACE('',#4988,1.);
#171=B_SPLINE_CURVE_WITH_KNOTS('',3,(#6538,#6539,#6540,#6541,#6542,#6543,
#6544,#6545,#6546,#6547,#6548,#6549),.UNSPECIFIED.,.F.,.F.,(4,2,2,2,2,4),
(-0.956775615070493,-0.896341583425285,-0.835907551780076,-0.715039488489658,
-0.596713648012452,-0.478387807535247),.UNSPECIFIED.);
#172=B_SPLINE_CURVE_WITH_KNOTS('',3,(#6550,#6551,#6552,#6553,#6554,#6555),
 .UNSPECIFIED.,.F.,.F.,(4,2,4),(-1.05899336181655,-1.0172096467157,-0.956775615070493),
 .UNSPECIFIED.);
#173=B_SPLINE_CURVE_WITH_KNOTS('',3,(#6557,#6558,#6559,#6560,#6561,#6562),
 .UNSPECIFIED.,.F.,.F.,(4,2,4),(0.956775615070494,1.0172096467157,1.0589933625076),
 .UNSPECIFIED.);
#174=B_SPLINE_CURVE_WITH_KNOTS('',3,(#6564,#6565,#6566,#6567,#6568,#6569,
#6570,#6571,#6572,#6573,#6574,#6575,#6576,#6577,#6578,#6579,#6580,#6581,
#6582,#6583,#6584,#6585,#6586,#6587,#6588,#6589,#6590),.UNSPECIFIED.,.F.,
 .F.,(4,2,3,2,2,2,2,2,2,2,2,2,4),(-0.102217746746059,-0.0604340316452088,
0.,0.0604340316452089,0.120868063290418,0.241736126580836,0.360061967058041,
0.478387807535247,0.596713648012453,0.715039488489658,0.835907551780076,
0.896341583425285,0.956775615070494),.UNSPECIFIED.);
#175=B_SPLINE_CURVE_WITH_KNOTS('',3,(#6593,#6594,#6595,#6596,#6597,#6598,
#6599,#6600,#6601,#6602,#6603,#6604,#6605,#6606,#6607,#6608,#6609),
 .UNSPECIFIED.,.F.,.F.,(4,2,2,2,2,3,2,4),(-0.478387807535247,-0.360061967058041,
-0.241736126580835,-0.120868063290418,-0.0604340316452086,2.22044604925031E-16,
0.0604340316452088,0.102217747437109),.UNSPECIFIED.);
#176=B_SPLINE_CURVE_WITH_KNOTS('',3,(#6630,#6631,#6632,#6633,#6634,#6635,
#6636,#6637,#6638,#6639,#6640,#6641),.UNSPECIFIED.,.F.,.F.,(4,2,2,2,2,4),
(-0.956775615070493,-0.896341583425285,-0.835907551780076,-0.715039488489658,
-0.596713648012452,-0.478387807535247),.UNSPECIFIED.);
#177=B_SPLINE_CURVE_WITH_KNOTS('',3,(#6642,#6643,#6644,#6645,#6646,#6647),
 .UNSPECIFIED.,.F.,.F.,(4,2,4),(-1.05899336181655,-1.0172096467157,-0.956775615070493),
 .UNSPECIFIED.);
#178=B_SPLINE_CURVE_WITH_KNOTS('',3,(#6649,#6650,#6651,#6652,#6653,#6654),
 .UNSPECIFIED.,.F.,.F.,(4,2,4),(0.956775615070493,1.0172096467157,1.0589933625076),
 .UNSPECIFIED.);
#179=B_SPLINE_CURVE_WITH_KNOTS('',3,(#6656,#6657,#6658,#6659,#6660,#6661,
#6662,#6663,#6664,#6665,#6666,#6667,#6668,#6669,#6670,#6671,#6672,#6673,
#6674,#6675,#6676,#6677,#6678,#6679,#6680,#6681,#6682),.UNSPECIFIED.,.F.,
 .F.,(4,2,3,2,2,2,2,2,2,2,2,2,4),(-0.102217746746057,-0.0604340316452088,
0.,0.0604340316452089,0.120868063290418,0.241736126580835,0.360061967058041,
0.478387807535247,0.596713648012452,0.715039488489658,0.835907551780075,
0.896341583425284,0.956775615070493),.UNSPECIFIED.);
#180=B_SPLINE_CURVE_WITH_KNOTS('',3,(#6685,#6686,#6687,#6688,#6689,#6690,
#6691,#6692,#6693,#6694,#6695,#6696,#6697,#6698,#6699,#6700,#6701),
 .UNSPECIFIED.,.F.,.F.,(4,2,2,2,2,3,2,4),(-0.478387807535247,-0.360061967058041,
-0.241736126580836,-0.120868063290418,-0.060434031645209,0.,0.0604340316452088,
0.102217747437111),.UNSPECIFIED.);
#181=B_SPLINE_CURVE_WITH_KNOTS('',3,(#6722,#6723,#6724,#6725,#6726,#6727,
#6728,#6729,#6730,#6731,#6732,#6733),.UNSPECIFIED.,.F.,.F.,(4,2,2,2,2,4),
(-0.956775615070493,-0.896341583425285,-0.835907551780076,-0.715039488489658,
-0.596713648012452,-0.478387807535247),.UNSPECIFIED.);
#182=B_SPLINE_CURVE_WITH_KNOTS('',3,(#6734,#6735,#6736,#6737,#6738,#6739),
 .UNSPECIFIED.,.F.,.F.,(4,2,4),(-1.05899336181655,-1.0172096467157,-0.956775615070493),
 .UNSPECIFIED.);
#183=B_SPLINE_CURVE_WITH_KNOTS('',3,(#6741,#6742,#6743,#6744,#6745,#6746),
 .UNSPECIFIED.,.F.,.F.,(4,2,4),(0.956775615070494,1.0172096467157,1.0589933625076),
 .UNSPECIFIED.);
#184=B_SPLINE_CURVE_WITH_KNOTS('',3,(#6748,#6749,#6750,#6751,#6752,#6753,
#6754,#6755,#6756,#6757,#6758,#6759,#6760,#6761,#6762,#6763,#6764,#6765,
#6766,#6767,#6768,#6769,#6770,#6771,#6772,#6773,#6774),.UNSPECIFIED.,.F.,
 .F.,(4,2,3,2,2,2,2,2,2,2,2,2,4),(-0.102217746746057,-0.0604340316452088,
0.,0.0604340316452089,0.120868063290418,0.241736126580836,0.360061967058041,
0.478387807535247,0.596713648012453,0.715039488489658,0.835907551780076,
0.896341583425285,0.956775615070494),.UNSPECIFIED.);
#185=B_SPLINE_CURVE_WITH_KNOTS('',3,(#6777,#6778,#6779,#6780,#6781,#6782,
#6783,#6784,#6785,#6786,#6787,#6788,#6789,#6790,#6791,#6792,#6793),
 .UNSPECIFIED.,.F.,.F.,(4,2,2,2,2,3,2,4),(-0.478387807535247,-0.360061967058041,
-0.241736126580835,-0.120868063290418,-0.0604340316452086,2.22044604925031E-16,
0.0604340316452088,0.102217747437111),.UNSPECIFIED.);
#186=B_SPLINE_CURVE_WITH_KNOTS('',3,(#6810,#6811,#6812,#6813,#6814,#6815,
#6816,#6817,#6818,#6819,#6820,#6821,#6822,#6823,#6824,#6825,#6826,#6827,
#6828,#6829,#6830,#6831,#6832,#6833,#6834,#6835,#6836,#6837,#6838,#6839,
#6840,#6841,#6842,#6843,#6844,#6845,#6846,#6847,#6848,#6849,#6850,#6851),
 .UNSPECIFIED.,.T.,.F.,(4,2,2,2,2,2,2,2,2,2,2,2,2,2,2,2,2,2,2,2,4),(0.,
0.0876674059984988,0.175334811996998,0.268557118055512,0.358098480537522,
0.447639843019532,0.537181205501541,0.626722567983551,0.719944874042066,
0.807612280040565,0.895279686039063,0.982947092037562,1.07061449803606,
1.16383680409458,1.25337816657659,1.3429195290586,1.43246089154061,1.52200225402261,
1.61522456008113,1.70289196607963,1.79055937207813),.UNSPECIFIED.);
#187=SHAPE_REPRESENTATION_RELATIONSHIP('SRR','None',#8001,#212);
#188=SHAPE_REPRESENTATION_RELATIONSHIP('SRR','None',#8002,#213);
#189=SHAPE_REPRESENTATION_RELATIONSHIP('SRR','None',#8003,#214);
#190=SHAPE_REPRESENTATION_RELATIONSHIP('SRR','None',#8004,#215);
#191=SHAPE_REPRESENTATION_RELATIONSHIP('SRR','None',#8005,#216);
#192=SHAPE_REPRESENTATION_RELATIONSHIP('SRR','None',#8006,#217);
#193=SHAPE_REPRESENTATION_RELATIONSHIP('SRR','None',#8007,#218);
#194=SHAPE_REPRESENTATION_RELATIONSHIP('SRR','None',#8008,#219);
#195=SHAPE_REPRESENTATION_RELATIONSHIP('SRR','None',#8009,#220);
#196=SHAPE_REPRESENTATION_RELATIONSHIP('SRR','None',#8010,#221);
#197=SHAPE_REPRESENTATION_RELATIONSHIP('SRR','None',#8011,#222);
#198=SHAPE_REPRESENTATION_RELATIONSHIP('SRR','None',#8012,#223);
#199=SHAPE_REPRESENTATION_RELATIONSHIP('SRR','None',#8013,#224);
#200=SHAPE_REPRESENTATION_RELATIONSHIP('SRR','None',#8014,#225);
#201=SHAPE_REPRESENTATION_RELATIONSHIP('SRR','None',#8016,#226);
#202=SHAPE_REPRESENTATION_RELATIONSHIP('SRR','None',#8017,#227);
#203=SHAPE_REPRESENTATION_RELATIONSHIP('SRR','None',#8018,#228);
#204=SHAPE_REPRESENTATION_RELATIONSHIP('SRR','None',#8020,#229);
#205=SHAPE_REPRESENTATION_RELATIONSHIP('SRR','None',#8021,#230);
#206=SHAPE_REPRESENTATION_RELATIONSHIP('SRR','None',#8022,#231);
#207=SHAPE_REPRESENTATION_RELATIONSHIP('SRR','None',#8024,#232);
#208=SHAPE_REPRESENTATION_RELATIONSHIP('SRR','None',#8025,#233);
#209=SHAPE_REPRESENTATION_RELATIONSHIP('SRR','None',#8026,#234);
#210=SHAPE_REPRESENTATION_RELATIONSHIP('SRR','None',#8028,#235);
#211=SHAPE_REPRESENTATION_RELATIONSHIP('SRR','None',#8029,#236);
#212=ADVANCED_BREP_SHAPE_REPRESENTATION('',(#262),#7868);
#213=ADVANCED_BREP_SHAPE_REPRESENTATION('',(#263),#7869);
#214=ADVANCED_BREP_SHAPE_REPRESENTATION('',(#264),#7870);
#215=ADVANCED_BREP_SHAPE_REPRESENTATION('',(#265),#7871);
#216=ADVANCED_BREP_SHAPE_REPRESENTATION('',(#266),#7872);
#217=ADVANCED_BREP_SHAPE_REPRESENTATION('',(#267),#7873);
#218=ADVANCED_BREP_SHAPE_REPRESENTATION('',(#268),#7874);
#219=ADVANCED_BREP_SHAPE_REPRESENTATION('',(#269),#7875);
#220=ADVANCED_BREP_SHAPE_REPRESENTATION('',(#270),#7876);
#221=ADVANCED_BREP_SHAPE_REPRESENTATION('',(#271),#7877);
#222=ADVANCED_BREP_SHAPE_REPRESENTATION('',(#272),#7878);
#223=ADVANCED_BREP_SHAPE_REPRESENTATION('',(#153),#7879);
#224=ADVANCED_BREP_SHAPE_REPRESENTATION('',(#154),#7880);
#225=ADVANCED_BREP_SHAPE_REPRESENTATION('',(#273),#7881);
#226=ADVANCED_BREP_SHAPE_REPRESENTATION('',(#274),#7883);
#227=ADVANCED_BREP_SHAPE_REPRESENTATION('',(#275),#7884);
#228=ADVANCED_BREP_SHAPE_REPRESENTATION('',(#276),#7885);
#229=ADVANCED_BREP_SHAPE_REPRESENTATION('',(#277),#7887);
#230=ADVANCED_BREP_SHAPE_REPRESENTATION('',(#278),#7888);
#231=ADVANCED_BREP_SHAPE_REPRESENTATION('',(#279),#7889);
#232=ADVANCED_BREP_SHAPE_REPRESENTATION('',(#280),#7891);
#233=ADVANCED_BREP_SHAPE_REPRESENTATION('',(#281),#7892);
#234=ADVANCED_BREP_SHAPE_REPRESENTATION('',(#282),#7893);
#235=ADVANCED_BREP_SHAPE_REPRESENTATION('',(#283),#7895);
#236=ADVANCED_BREP_SHAPE_REPRESENTATION('',(#284),#7896);
#237=STYLED_ITEM('',(#8199),#262);
#238=STYLED_ITEM('',(#8213),#263);
#239=STYLED_ITEM('',(#8213),#264);
#240=STYLED_ITEM('',(#8234),#265);
#241=STYLED_ITEM('',(#8234),#266);
#242=STYLED_ITEM('',(#8213),#267);
#243=STYLED_ITEM('',(#8227),#268);
#244=STYLED_ITEM('',(#8227),#269);
#245=STYLED_ITEM('',(#8227),#270);
#246=STYLED_ITEM('',(#8234),#271);
#247=STYLED_ITEM('',(#8227),#272);
#248=STYLED_ITEM('',(#8227),#153);
#249=STYLED_ITEM('',(#8227),#154);
#250=STYLED_ITEM('',(#8213),#273);
#251=STYLED_ITEM('',(#8234),#274);
#252=STYLED_ITEM('',(#8206),#275);
#253=STYLED_ITEM('',(#8213),#276);
#254=STYLED_ITEM('',(#8234),#277);
#255=STYLED_ITEM('',(#8206),#278);
#256=STYLED_ITEM('',(#8213),#279);
#257=STYLED_ITEM('',(#8234),#280);
#258=STYLED_ITEM('',(#8206),#281);
#259=STYLED_ITEM('',(#8213),#282);
#260=STYLED_ITEM('',(#8199),#283);
#261=STYLED_ITEM('',(#8234),#284);
#262=MANIFOLD_SOLID_BREP('Body1',#4286);
#263=MANIFOLD_SOLID_BREP('Body1',#4287);
#264=MANIFOLD_SOLID_BREP('Body1',#4288);
#265=MANIFOLD_SOLID_BREP('Body1',#4289);
#266=MANIFOLD_SOLID_BREP('Body1',#4290);
#267=MANIFOLD_SOLID_BREP('Body1',#4291);
#268=MANIFOLD_SOLID_BREP('Body1',#4292);
#269=MANIFOLD_SOLID_BREP('Body1',#4293);
#270=MANIFOLD_SOLID_BREP('Body1',#4294);
#271=MANIFOLD_SOLID_BREP('Body1',#4295);
#272=MANIFOLD_SOLID_BREP('Body1',#4296);
#273=MANIFOLD_SOLID_BREP('Body1',#4301);
#274=MANIFOLD_SOLID_BREP('Body1',#4302);
#275=MANIFOLD_SOLID_BREP('Body1',#4303);
#276=MANIFOLD_SOLID_BREP('Body1',#4304);
#277=MANIFOLD_SOLID_BREP('Body1',#4305);
#278=MANIFOLD_SOLID_BREP('Body1',#4306);
#279=MANIFOLD_SOLID_BREP('Body1',#4307);
#280=MANIFOLD_SOLID_BREP('Body1',#4308);
#281=MANIFOLD_SOLID_BREP('Body1',#4309);
#282=MANIFOLD_SOLID_BREP('Body1',#4310);
#283=MANIFOLD_SOLID_BREP('Body1',#4311);
#284=MANIFOLD_SOLID_BREP('Body1',#4312);
#285=FACE_BOUND('',#802,.T.);
#286=FACE_BOUND('',#804,.T.);
#287=FACE_BOUND('',#825,.T.);
#288=FACE_BOUND('',#826,.T.);
#289=FACE_BOUND('',#827,.T.);
#290=FACE_BOUND('',#829,.T.);
#291=FACE_BOUND('',#830,.T.);
#292=FACE_BOUND('',#831,.T.);
#293=FACE_BOUND('',#837,.T.);
#294=FACE_BOUND('',#843,.T.);
#295=FACE_BOUND('',#849,.T.);
#296=FACE_BOUND('',#851,.T.);
#297=FACE_BOUND('',#853,.T.);
#298=FACE_BOUND('',#857,.T.);
#299=FACE_BOUND('',#859,.T.);
#300=FACE_BOUND('',#861,.T.);
#301=FACE_BOUND('',#866,.T.);
#302=FACE_BOUND('',#868,.T.);
#303=FACE_BOUND('',#869,.T.);
#304=FACE_BOUND('',#870,.T.);
#305=FACE_BOUND('',#872,.T.);
#306=FACE_BOUND('',#874,.T.);
#307=FACE_BOUND('',#875,.T.);
#308=FACE_BOUND('',#877,.T.);
#309=FACE_BOUND('',#878,.T.);
#310=FACE_BOUND('',#885,.T.);
#311=FACE_BOUND('',#886,.T.);
#312=FACE_BOUND('',#889,.T.);
#313=FACE_BOUND('',#892,.T.);
#314=FACE_BOUND('',#894,.T.);
#315=FACE_BOUND('',#898,.T.);
#316=FACE_BOUND('',#899,.T.);
#317=FACE_BOUND('',#902,.T.);
#318=FACE_BOUND('',#905,.T.);
#319=FACE_BOUND('',#907,.T.);
#320=FACE_BOUND('',#911,.T.);
#321=FACE_BOUND('',#912,.T.);
#322=FACE_BOUND('',#915,.T.);
#323=FACE_BOUND('',#918,.T.);
#324=FACE_BOUND('',#920,.T.);
#325=FACE_BOUND('',#967,.T.);
#326=FACE_BOUND('',#969,.T.);
#327=FACE_BOUND('',#973,.T.);
#328=FACE_BOUND('',#976,.T.);
#329=FACE_BOUND('',#991,.T.);
#330=FACE_BOUND('',#999,.T.);
#331=FACE_BOUND('',#1013,.T.);
#332=FACE_BOUND('',#1015,.T.);
#333=FACE_BOUND('',#1024,.T.);
#334=FACE_BOUND('',#1029,.T.);
#335=FACE_BOUND('',#1033,.T.);
#336=FACE_BOUND('',#1037,.T.);
#337=FACE_BOUND('',#1039,.T.);
#338=FACE_BOUND('',#1040,.T.);
#339=FACE_BOUND('',#1044,.T.);
#340=FACE_BOUND('',#1046,.T.);
#341=FACE_BOUND('',#1049,.T.);
#342=FACE_BOUND('',#1053,.T.);
#343=FACE_BOUND('',#1055,.T.);
#344=FACE_BOUND('',#1058,.T.);
#345=FACE_BOUND('',#1062,.T.);
#346=FACE_BOUND('',#1064,.T.);
#347=FACE_BOUND('',#1065,.T.);
#348=FACE_BOUND('',#1069,.T.);
#349=FACE_BOUND('',#1071,.T.);
#350=FACE_BOUND('',#1074,.T.);
#351=FACE_BOUND('',#1078,.T.);
#352=FACE_BOUND('',#1080,.T.);
#353=FACE_BOUND('',#1083,.T.);
#354=FACE_BOUND('',#1087,.T.);
#355=FACE_BOUND('',#1089,.T.);
#356=FACE_BOUND('',#1090,.T.);
#357=FACE_BOUND('',#1094,.T.);
#358=FACE_BOUND('',#1096,.T.);
#359=FACE_BOUND('',#1099,.T.);
#360=FACE_BOUND('',#1103,.T.);
#361=FACE_BOUND('',#1105,.T.);
#362=FACE_BOUND('',#1108,.T.);
#363=FACE_BOUND('',#1110,.T.);
#364=FACE_BOUND('',#1112,.T.);
#365=FACE_BOUND('',#1120,.T.);
#366=FACE_BOUND('',#1123,.T.);
#367=FACE_BOUND('',#1127,.T.);
#368=FACE_BOUND('',#1130,.T.);
#369=FACE_BOUND('',#1133,.T.);
#370=FACE_BOUND('',#1136,.T.);
#371=PLANE('',#4595);
#372=PLANE('',#4596);
#373=PLANE('',#4597);
#374=PLANE('',#4598);
#375=PLANE('',#4599);
#376=PLANE('',#4600);
#377=PLANE('',#4602);
#378=PLANE('',#4603);
#379=PLANE('',#4604);
#380=PLANE('',#4605);
#381=PLANE('',#4606);
#382=PLANE('',#4607);
#383=PLANE('',#4609);
#384=PLANE('',#4610);
#385=PLANE('',#4611);
#386=PLANE('',#4612);
#387=PLANE('',#4613);
#388=PLANE('',#4614);
#389=PLANE('',#4625);
#390=PLANE('',#4626);
#391=PLANE('',#4627);
#392=PLANE('',#4628);
#393=PLANE('',#4629);
#394=PLANE('',#4630);
#395=PLANE('',#4632);
#396=PLANE('',#4637);
#397=PLANE('',#4641);
#398=PLANE('',#4642);
#399=PLANE('',#4647);
#400=PLANE('',#4651);
#401=PLANE('',#4652);
#402=PLANE('',#4657);
#403=PLANE('',#4661);
#404=PLANE('',#4665);
#405=PLANE('',#4672);
#406=PLANE('',#4677);
#407=PLANE('',#4683);
#408=PLANE('',#4684);
#409=PLANE('',#4685);
#410=PLANE('',#4686);
#411=PLANE('',#4687);
#412=PLANE('',#4688);
#413=PLANE('',#4693);
#414=PLANE('',#4694);
#415=PLANE('',#4707);
#416=PLANE('',#4711);
#417=PLANE('',#4712);
#418=PLANE('',#4725);
#419=PLANE('',#4729);
#420=PLANE('',#4730);
#421=PLANE('',#4743);
#422=PLANE('',#4747);
#423=PLANE('',#4748);
#424=PLANE('',#4750);
#425=PLANE('',#4751);
#426=PLANE('',#4752);
#427=PLANE('',#4753);
#428=PLANE('',#4754);
#429=PLANE('',#4755);
#430=PLANE('',#4756);
#431=PLANE('',#4757);
#432=PLANE('',#4758);
#433=PLANE('',#4759);
#434=PLANE('',#4760);
#435=PLANE('',#4761);
#436=PLANE('',#4762);
#437=PLANE('',#4763);
#438=PLANE('',#4764);
#439=PLANE('',#4765);
#440=PLANE('',#4766);
#441=PLANE('',#4767);
#442=PLANE('',#4768);
#443=PLANE('',#4769);
#444=PLANE('',#4770);
#445=PLANE('',#4771);
#446=PLANE('',#4772);
#447=PLANE('',#4773);
#448=PLANE('',#4774);
#449=PLANE('',#4775);
#450=PLANE('',#4776);
#451=PLANE('',#4777);
#452=PLANE('',#4778);
#453=PLANE('',#4779);
#454=PLANE('',#4780);
#455=PLANE('',#4781);
#456=PLANE('',#4782);
#457=PLANE('',#4783);
#458=PLANE('',#4784);
#459=PLANE('',#4785);
#460=PLANE('',#4789);
#461=PLANE('',#4790);
#462=PLANE('',#4791);
#463=PLANE('',#4792);
#464=PLANE('',#4793);
#465=PLANE('',#4794);
#466=PLANE('',#4795);
#467=PLANE('',#4796);
#468=PLANE('',#4797);
#469=PLANE('',#4798);
#470=PLANE('',#4805);
#471=PLANE('',#4809);
#472=PLANE('',#4811);
#473=PLANE('',#4812);
#474=PLANE('',#4813);
#475=PLANE('',#4814);
#476=PLANE('',#4815);
#477=PLANE('',#4816);
#478=PLANE('',#4817);
#479=PLANE('',#4818);
#480=PLANE('',#4819);
#481=PLANE('',#4821);
#482=PLANE('',#4829);
#483=PLANE('',#4835);
#484=PLANE('',#4843);
#485=PLANE('',#4851);
#486=PLANE('',#4852);
#487=PLANE('',#4853);
#488=PLANE('',#4854);
#489=PLANE('',#4855);
#490=PLANE('',#4856);
#491=PLANE('',#4857);
#492=PLANE('',#4858);
#493=PLANE('',#4859);
#494=PLANE('',#4861);
#495=PLANE('',#4863);
#496=PLANE('',#4865);
#497=PLANE('',#4866);
#498=PLANE('',#4867);
#499=PLANE('',#4868);
#500=PLANE('',#4869);
#501=PLANE('',#4870);
#502=PLANE('',#4873);
#503=PLANE('',#4881);
#504=PLANE('',#4906);
#505=PLANE('',#4913);
#506=PLANE('',#4923);
#507=PLANE('',#4924);
#508=PLANE('',#4929);
#509=PLANE('',#4936);
#510=PLANE('',#4937);
#511=PLANE('',#4943);
#512=PLANE('',#4950);
#513=PLANE('',#4960);
#514=PLANE('',#4961);
#515=PLANE('',#4966);
#516=PLANE('',#4973);
#517=PLANE('',#4974);
#518=PLANE('',#4980);
#519=PLANE('',#4987);
#520=PLANE('',#4997);
#521=PLANE('',#4998);
#522=PLANE('',#5003);
#523=PLANE('',#5010);
#524=PLANE('',#5011);
#525=PLANE('',#5017);
#526=PLANE('',#5019);
#527=PLANE('',#5021);
#528=PLANE('',#5023);
#529=PLANE('',#5024);
#530=PLANE('',#5025);
#531=PLANE('',#5026);
#532=PLANE('',#5027);
#533=PLANE('',#5028);
#534=PLANE('',#5029);
#535=PLANE('',#5033);
#536=PLANE('',#5038);
#537=PLANE('',#5042);
#538=PLANE('',#5047);
#539=PLANE('',#5051);
#540=FACE_OUTER_BOUND('',#796,.T.);
#541=FACE_OUTER_BOUND('',#797,.T.);
#542=FACE_OUTER_BOUND('',#798,.T.);
#543=FACE_OUTER_BOUND('',#799,.T.);
#544=FACE_OUTER_BOUND('',#800,.T.);
#545=FACE_OUTER_BOUND('',#801,.T.);
#546=FACE_OUTER_BOUND('',#803,.T.);
#547=FACE_OUTER_BOUND('',#805,.T.);
#548=FACE_OUTER_BOUND('',#806,.T.);
#549=FACE_OUTER_BOUND('',#807,.T.);
#550=FACE_OUTER_BOUND('',#808,.T.);
#551=FACE_OUTER_BOUND('',#809,.T.);
#552=FACE_OUTER_BOUND('',#810,.T.);
#553=FACE_OUTER_BOUND('',#811,.T.);
#554=FACE_OUTER_BOUND('',#812,.T.);
#555=FACE_OUTER_BOUND('',#813,.T.);
#556=FACE_OUTER_BOUND('',#814,.T.);
#557=FACE_OUTER_BOUND('',#815,.T.);
#558=FACE_OUTER_BOUND('',#816,.T.);
#559=FACE_OUTER_BOUND('',#817,.T.);
#560=FACE_OUTER_BOUND('',#818,.T.);
#561=FACE_OUTER_BOUND('',#819,.T.);
#562=FACE_OUTER_BOUND('',#820,.T.);
#563=FACE_OUTER_BOUND('',#821,.T.);
#564=FACE_OUTER_BOUND('',#822,.T.);
#565=FACE_OUTER_BOUND('',#823,.T.);
#566=FACE_OUTER_BOUND('',#824,.T.);
#567=FACE_OUTER_BOUND('',#828,.T.);
#568=FACE_OUTER_BOUND('',#832,.T.);
#569=FACE_OUTER_BOUND('',#833,.T.);
#570=FACE_OUTER_BOUND('',#834,.T.);
#571=FACE_OUTER_BOUND('',#835,.T.);
#572=FACE_OUTER_BOUND('',#836,.T.);
#573=FACE_OUTER_BOUND('',#838,.T.);
#574=FACE_OUTER_BOUND('',#839,.T.);
#575=FACE_OUTER_BOUND('',#840,.T.);
#576=FACE_OUTER_BOUND('',#841,.T.);
#577=FACE_OUTER_BOUND('',#842,.T.);
#578=FACE_OUTER_BOUND('',#844,.T.);
#579=FACE_OUTER_BOUND('',#845,.T.);
#580=FACE_OUTER_BOUND('',#846,.T.);
#581=FACE_OUTER_BOUND('',#847,.T.);
#582=FACE_OUTER_BOUND('',#848,.T.);
#583=FACE_OUTER_BOUND('',#850,.T.);
#584=FACE_OUTER_BOUND('',#852,.T.);
#585=FACE_OUTER_BOUND('',#854,.T.);
#586=FACE_OUTER_BOUND('',#855,.T.);
#587=FACE_OUTER_BOUND('',#856,.T.);
#588=FACE_OUTER_BOUND('',#858,.T.);
#589=FACE_OUTER_BOUND('',#860,.T.);
#590=FACE_OUTER_BOUND('',#862,.T.);
#591=FACE_OUTER_BOUND('',#863,.T.);
#592=FACE_OUTER_BOUND('',#864,.T.);
#593=FACE_OUTER_BOUND('',#865,.T.);
#594=FACE_OUTER_BOUND('',#867,.T.);
#595=FACE_OUTER_BOUND('',#871,.T.);
#596=FACE_OUTER_BOUND('',#873,.T.);
#597=FACE_OUTER_BOUND('',#876,.T.);
#598=FACE_OUTER_BOUND('',#879,.T.);
#599=FACE_OUTER_BOUND('',#880,.T.);
#600=FACE_OUTER_BOUND('',#881,.T.);
#601=FACE_OUTER_BOUND('',#882,.T.);
#602=FACE_OUTER_BOUND('',#883,.T.);
#603=FACE_OUTER_BOUND('',#884,.T.);
#604=FACE_OUTER_BOUND('',#887,.T.);
#605=FACE_OUTER_BOUND('',#888,.T.);
#606=FACE_OUTER_BOUND('',#890,.T.);
#607=FACE_OUTER_BOUND('',#891,.T.);
#608=FACE_OUTER_BOUND('',#893,.T.);
#609=FACE_OUTER_BOUND('',#895,.T.);
#610=FACE_OUTER_BOUND('',#896,.T.);
#611=FACE_OUTER_BOUND('',#897,.T.);
#612=FACE_OUTER_BOUND('',#900,.T.);
#613=FACE_OUTER_BOUND('',#901,.T.);
#614=FACE_OUTER_BOUND('',#903,.T.);
#615=FACE_OUTER_BOUND('',#904,.T.);
#616=FACE_OUTER_BOUND('',#906,.T.);
#617=FACE_OUTER_BOUND('',#908,.T.);
#618=FACE_OUTER_BOUND('',#909,.T.);
#619=FACE_OUTER_BOUND('',#910,.T.);
#620=FACE_OUTER_BOUND('',#913,.T.);
#621=FACE_OUTER_BOUND('',#914,.T.);
#622=FACE_OUTER_BOUND('',#916,.T.);
#623=FACE_OUTER_BOUND('',#917,.T.);
#624=FACE_OUTER_BOUND('',#919,.T.);
#625=FACE_OUTER_BOUND('',#921,.T.);
#626=FACE_OUTER_BOUND('',#922,.T.);
#627=FACE_OUTER_BOUND('',#923,.T.);
#628=FACE_OUTER_BOUND('',#924,.T.);
#629=FACE_OUTER_BOUND('',#925,.T.);
#630=FACE_OUTER_BOUND('',#926,.T.);
#631=FACE_OUTER_BOUND('',#927,.T.);
#632=FACE_OUTER_BOUND('',#928,.T.);
#633=FACE_OUTER_BOUND('',#929,.T.);
#634=FACE_OUTER_BOUND('',#930,.T.);
#635=FACE_OUTER_BOUND('',#931,.T.);
#636=FACE_OUTER_BOUND('',#932,.T.);
#637=FACE_OUTER_BOUND('',#933,.T.);
#638=FACE_OUTER_BOUND('',#934,.T.);
#639=FACE_OUTER_BOUND('',#935,.T.);
#640=FACE_OUTER_BOUND('',#936,.T.);
#641=FACE_OUTER_BOUND('',#937,.T.);
#642=FACE_OUTER_BOUND('',#938,.T.);
#643=FACE_OUTER_BOUND('',#939,.T.);
#644=FACE_OUTER_BOUND('',#940,.T.);
#645=FACE_OUTER_BOUND('',#941,.T.);
#646=FACE_OUTER_BOUND('',#942,.T.);
#647=FACE_OUTER_BOUND('',#943,.T.);
#648=FACE_OUTER_BOUND('',#944,.T.);
#649=FACE_OUTER_BOUND('',#945,.T.);
#650=FACE_OUTER_BOUND('',#946,.T.);
#651=FACE_OUTER_BOUND('',#947,.T.);
#652=FACE_OUTER_BOUND('',#948,.T.);
#653=FACE_OUTER_BOUND('',#949,.T.);
#654=FACE_OUTER_BOUND('',#950,.T.);
#655=FACE_OUTER_BOUND('',#951,.T.);
#656=FACE_OUTER_BOUND('',#952,.T.);
#657=FACE_OUTER_BOUND('',#953,.T.);
#658=FACE_OUTER_BOUND('',#954,.T.);
#659=FACE_OUTER_BOUND('',#955,.T.);
#660=FACE_OUTER_BOUND('',#956,.T.);
#661=FACE_OUTER_BOUND('',#957,.T.);
#662=FACE_OUTER_BOUND('',#958,.T.);
#663=FACE_OUTER_BOUND('',#959,.T.);
#664=FACE_OUTER_BOUND('',#960,.T.);
#665=FACE_OUTER_BOUND('',#961,.T.);
#666=FACE_OUTER_BOUND('',#962,.T.);
#667=FACE_OUTER_BOUND('',#963,.T.);
#668=FACE_OUTER_BOUND('',#964,.T.);
#669=FACE_OUTER_BOUND('',#965,.T.);
#670=FACE_OUTER_BOUND('',#966,.T.);
#671=FACE_OUTER_BOUND('',#968,.T.);
#672=FACE_OUTER_BOUND('',#970,.T.);
#673=FACE_OUTER_BOUND('',#971,.T.);
#674=FACE_OUTER_BOUND('',#972,.T.);
#675=FACE_OUTER_BOUND('',#974,.T.);
#676=FACE_OUTER_BOUND('',#975,.T.);
#677=FACE_OUTER_BOUND('',#977,.T.);
#678=FACE_OUTER_BOUND('',#978,.T.);
#679=FACE_OUTER_BOUND('',#979,.T.);
#680=FACE_OUTER_BOUND('',#980,.T.);
#681=FACE_OUTER_BOUND('',#981,.T.);
#682=FACE_OUTER_BOUND('',#982,.T.);
#683=FACE_OUTER_BOUND('',#983,.T.);
#684=FACE_OUTER_BOUND('',#984,.T.);
#685=FACE_OUTER_BOUND('',#985,.T.);
#686=FACE_OUTER_BOUND('',#986,.T.);
#687=FACE_OUTER_BOUND('',#987,.T.);
#688=FACE_OUTER_BOUND('',#988,.T.);
#689=FACE_OUTER_BOUND('',#989,.T.);
#690=FACE_OUTER_BOUND('',#990,.T.);
#691=FACE_OUTER_BOUND('',#992,.T.);
#692=FACE_OUTER_BOUND('',#993,.T.);
#693=FACE_OUTER_BOUND('',#994,.T.);
#694=FACE_OUTER_BOUND('',#995,.T.);
#695=FACE_OUTER_BOUND('',#996,.T.);
#696=FACE_OUTER_BOUND('',#997,.T.);
#697=FACE_OUTER_BOUND('',#998,.T.);
#698=FACE_OUTER_BOUND('',#1000,.T.);
#699=FACE_OUTER_BOUND('',#1001,.T.);
#700=FACE_OUTER_BOUND('',#1002,.T.);
#701=FACE_OUTER_BOUND('',#1003,.T.);
#702=FACE_OUTER_BOUND('',#1004,.T.);
#703=FACE_OUTER_BOUND('',#1005,.T.);
#704=FACE_OUTER_BOUND('',#1006,.T.);
#705=FACE_OUTER_BOUND('',#1007,.T.);
#706=FACE_OUTER_BOUND('',#1008,.T.);
#707=FACE_OUTER_BOUND('',#1009,.T.);
#708=FACE_OUTER_BOUND('',#1010,.T.);
#709=FACE_OUTER_BOUND('',#1011,.T.);
#710=FACE_OUTER_BOUND('',#1012,.T.);
#711=FACE_OUTER_BOUND('',#1014,.T.);
#712=FACE_OUTER_BOUND('',#1016,.T.);
#713=FACE_OUTER_BOUND('',#1017,.T.);
#714=FACE_OUTER_BOUND('',#1018,.T.);
#715=FACE_OUTER_BOUND('',#1019,.T.);
#716=FACE_OUTER_BOUND('',#1020,.T.);
#717=FACE_OUTER_BOUND('',#1021,.T.);
#718=FACE_OUTER_BOUND('',#1022,.T.);
#719=FACE_OUTER_BOUND('',#1023,.T.);
#720=FACE_OUTER_BOUND('',#1025,.T.);
#721=FACE_OUTER_BOUND('',#1026,.T.);
#722=FACE_OUTER_BOUND('',#1027,.T.);
#723=FACE_OUTER_BOUND('',#1028,.T.);
#724=FACE_OUTER_BOUND('',#1030,.T.);
#725=FACE_OUTER_BOUND('',#1031,.T.);
#726=FACE_OUTER_BOUND('',#1032,.T.);
#727=FACE_OUTER_BOUND('',#1034,.T.);
#728=FACE_OUTER_BOUND('',#1035,.T.);
#729=FACE_OUTER_BOUND('',#1036,.T.);
#730=FACE_OUTER_BOUND('',#1038,.T.);
#731=FACE_OUTER_BOUND('',#1041,.T.);
#732=FACE_OUTER_BOUND('',#1042,.T.);
#733=FACE_OUTER_BOUND('',#1043,.T.);
#734=FACE_OUTER_BOUND('',#1045,.T.);
#735=FACE_OUTER_BOUND('',#1047,.T.);
#736=FACE_OUTER_BOUND('',#1048,.T.);
#737=FACE_OUTER_BOUND('',#1050,.T.);
#738=FACE_OUTER_BOUND('',#1051,.T.);
#739=FACE_OUTER_BOUND('',#1052,.T.);
#740=FACE_OUTER_BOUND('',#1054,.T.);
#741=FACE_OUTER_BOUND('',#1056,.T.);
#742=FACE_OUTER_BOUND('',#1057,.T.);
#743=FACE_OUTER_BOUND('',#1059,.T.);
#744=FACE_OUTER_BOUND('',#1060,.T.);
#745=FACE_OUTER_BOUND('',#1061,.T.);
#746=FACE_OUTER_BOUND('',#1063,.T.);
#747=FACE_OUTER_BOUND('',#1066,.T.);
#748=FACE_OUTER_BOUND('',#1067,.T.);
#749=FACE_OUTER_BOUND('',#1068,.T.);
#750=FACE_OUTER_BOUND('',#1070,.T.);
#751=FACE_OUTER_BOUND('',#1072,.T.);
#752=FACE_OUTER_BOUND('',#1073,.T.);
#753=FACE_OUTER_BOUND('',#1075,.T.);
#754=FACE_OUTER_BOUND('',#1076,.T.);
#755=FACE_OUTER_BOUND('',#1077,.T.);
#756=FACE_OUTER_BOUND('',#1079,.T.);
#757=FACE_OUTER_BOUND('',#1081,.T.);
#758=FACE_OUTER_BOUND('',#1082,.T.);
#759=FACE_OUTER_BOUND('',#1084,.T.);
#760=FACE_OUTER_BOUND('',#1085,.T.);
#761=FACE_OUTER_BOUND('',#1086,.T.);
#762=FACE_OUTER_BOUND('',#1088,.T.);
#763=FACE_OUTER_BOUND('',#1091,.T.);
#764=FACE_OUTER_BOUND('',#1092,.T.);
#765=FACE_OUTER_BOUND('',#1093,.T.);
#766=FACE_OUTER_BOUND('',#1095,.T.);
#767=FACE_OUTER_BOUND('',#1097,.T.);
#768=FACE_OUTER_BOUND('',#1098,.T.);
#769=FACE_OUTER_BOUND('',#1100,.T.);
#770=FACE_OUTER_BOUND('',#1101,.T.);
#771=FACE_OUTER_BOUND('',#1102,.T.);
#772=FACE_OUTER_BOUND('',#1104,.T.);
#773=FACE_OUTER_BOUND('',#1106,.T.);
#774=FACE_OUTER_BOUND('',#1107,.T.);
#775=FACE_OUTER_BOUND('',#1109,.T.);
#776=FACE_OUTER_BOUND('',#1111,.T.);
#777=FACE_OUTER_BOUND('',#1113,.T.);
#778=FACE_OUTER_BOUND('',#1114,.T.);
#779=FACE_OUTER_BOUND('',#1115,.T.);
#780=FACE_OUTER_BOUND('',#1116,.T.);
#781=FACE_OUTER_BOUND('',#1117,.T.);
#782=FACE_OUTER_BOUND('',#1118,.T.);
#783=FACE_OUTER_BOUND('',#1119,.T.);
#784=FACE_OUTER_BOUND('',#1121,.T.);
#785=FACE_OUTER_BOUND('',#1122,.T.);
#786=FACE_OUTER_BOUND('',#1124,.T.);
#787=FACE_OUTER_BOUND('',#1125,.T.);
#788=FACE_OUTER_BOUND('',#1126,.T.);
#789=FACE_OUTER_BOUND('',#1128,.T.);
#790=FACE_OUTER_BOUND('',#1129,.T.);
#791=FACE_OUTER_BOUND('',#1131,.T.);
#792=FACE_OUTER_BOUND('',#1132,.T.);
#793=FACE_OUTER_BOUND('',#1134,.T.);
#794=FACE_OUTER_BOUND('',#1135,.T.);
#795=FACE_OUTER_BOUND('',#1137,.T.);
#796=EDGE_LOOP('',(#2897,#2898,#2899,#2900));
#797=EDGE_LOOP('',(#2901,#2902,#2903,#2904));
#798=EDGE_LOOP('',(#2905,#2906,#2907,#2908));
#799=EDGE_LOOP('',(#2909,#2910,#2911,#2912));
#800=EDGE_LOOP('',(#2913,#2914,#2915,#2916));
#801=EDGE_LOOP('',(#2917,#2918,#2919,#2920));
#802=EDGE_LOOP('',(#2921));
#803=EDGE_LOOP('',(#2922,#2923,#2924,#2925));
#804=EDGE_LOOP('',(#2926));
#805=EDGE_LOOP('',(#2927,#2928,#2929,#2930));
#806=EDGE_LOOP('',(#2931,#2932,#2933,#2934));
#807=EDGE_LOOP('',(#2935,#2936,#2937,#2938));
#808=EDGE_LOOP('',(#2939,#2940,#2941,#2942));
#809=EDGE_LOOP('',(#2943,#2944,#2945,#2946));
#810=EDGE_LOOP('',(#2947,#2948,#2949,#2950));
#811=EDGE_LOOP('',(#2951,#2952,#2953,#2954));
#812=EDGE_LOOP('',(#2955,#2956,#2957,#2958));
#813=EDGE_LOOP('',(#2959,#2960,#2961,#2962));
#814=EDGE_LOOP('',(#2963,#2964,#2965,#2966));
#815=EDGE_LOOP('',(#2967,#2968,#2969,#2970));
#816=EDGE_LOOP('',(#2971,#2972,#2973,#2974));
#817=EDGE_LOOP('',(#2975,#2976,#2977,#2978));
#818=EDGE_LOOP('',(#2979,#2980,#2981,#2982));
#819=EDGE_LOOP('',(#2983,#2984,#2985,#2986));
#820=EDGE_LOOP('',(#2987,#2988,#2989,#2990));
#821=EDGE_LOOP('',(#2991,#2992,#2993,#2994));
#822=EDGE_LOOP('',(#2995,#2996,#2997,#2998));
#823=EDGE_LOOP('',(#2999,#3000,#3001,#3002));
#824=EDGE_LOOP('',(#3003,#3004,#3005,#3006));
#825=EDGE_LOOP('',(#3007));
#826=EDGE_LOOP('',(#3008));
#827=EDGE_LOOP('',(#3009));
#828=EDGE_LOOP('',(#3010,#3011,#3012,#3013));
#829=EDGE_LOOP('',(#3014));
#830=EDGE_LOOP('',(#3015));
#831=EDGE_LOOP('',(#3016));
#832=EDGE_LOOP('',(#3017,#3018));
#833=EDGE_LOOP('',(#3019,#3020,#3021,#3022,#3023,#3024,#3025,#3026,#3027,
#3028));
#834=EDGE_LOOP('',(#3029,#3030));
#835=EDGE_LOOP('',(#3031,#3032,#3033,#3034));
#836=EDGE_LOOP('',(#3035));
#837=EDGE_LOOP('',(#3036));
#838=EDGE_LOOP('',(#3037,#3038));
#839=EDGE_LOOP('',(#3039,#3040,#3041,#3042,#3043,#3044,#3045,#3046,#3047,
#3048));
#840=EDGE_LOOP('',(#3049,#3050));
#841=EDGE_LOOP('',(#3051,#3052,#3053,#3054));
#842=EDGE_LOOP('',(#3055));
#843=EDGE_LOOP('',(#3056));
#844=EDGE_LOOP('',(#3057,#3058));
#845=EDGE_LOOP('',(#3059,#3060,#3061,#3062,#3063,#3064,#3065,#3066,#3067,
#3068));
#846=EDGE_LOOP('',(#3069,#3070));
#847=EDGE_LOOP('',(#3071,#3072,#3073,#3074));
#848=EDGE_LOOP('',(#3075));
#849=EDGE_LOOP('',(#3076));
#850=EDGE_LOOP('',(#3077,#3078,#3079,#3080));
#851=EDGE_LOOP('',(#3081));
#852=EDGE_LOOP('',(#3082));
#853=EDGE_LOOP('',(#3083));
#854=EDGE_LOOP('',(#3084,#3085,#3086,#3087,#3088,#3089,#3090,#3091,#3092,
#3093,#3094,#3095,#3096,#3097,#3098,#3099,#3100,#3101,#3102,#3103,#3104,
#3105,#3106,#3107,#3108,#3109,#3110,#3111,#3112,#3113,#3114));
#855=EDGE_LOOP('',(#3115,#3116,#3117,#3118));
#856=EDGE_LOOP('',(#3119));
#857=EDGE_LOOP('',(#3120));
#858=EDGE_LOOP('',(#3121,#3122,#3123,#3124));
#859=EDGE_LOOP('',(#3125));
#860=EDGE_LOOP('',(#3126));
#861=EDGE_LOOP('',(#3127));
#862=EDGE_LOOP('',(#3128,#3129,#3130,#3131));
#863=EDGE_LOOP('',(#3132,#3133,#3134,#3135));
#864=EDGE_LOOP('',(#3136,#3137,#3138,#3139));
#865=EDGE_LOOP('',(#3140,#3141,#3142,#3143));
#866=EDGE_LOOP('',(#3144));
#867=EDGE_LOOP('',(#3145,#3146,#3147,#3148));
#868=EDGE_LOOP('',(#3149));
#869=EDGE_LOOP('',(#3150));
#870=EDGE_LOOP('',(#3151));
#871=EDGE_LOOP('',(#3152,#3153,#3154,#3155));
#872=EDGE_LOOP('',(#3156));
#873=EDGE_LOOP('',(#3157,#3158,#3159,#3160));
#874=EDGE_LOOP('',(#3161));
#875=EDGE_LOOP('',(#3162));
#876=EDGE_LOOP('',(#3163,#3164,#3165,#3166));
#877=EDGE_LOOP('',(#3167));
#878=EDGE_LOOP('',(#3168));
#879=EDGE_LOOP('',(#3169,#3170,#3171,#3172));
#880=EDGE_LOOP('',(#3173));
#881=EDGE_LOOP('',(#3174));
#882=EDGE_LOOP('',(#3175,#3176,#3177,#3178));
#883=EDGE_LOOP('',(#3179,#3180,#3181,#3182));
#884=EDGE_LOOP('',(#3183,#3184));
#885=EDGE_LOOP('',(#3185));
#886=EDGE_LOOP('',(#3186));
#887=EDGE_LOOP('',(#3187,#3188,#3189,#3190));
#888=EDGE_LOOP('',(#3191));
#889=EDGE_LOOP('',(#3192));
#890=EDGE_LOOP('',(#3193,#3194,#3195,#3196));
#891=EDGE_LOOP('',(#3197));
#892=EDGE_LOOP('',(#3198));
#893=EDGE_LOOP('',(#3199));
#894=EDGE_LOOP('',(#3200));
#895=EDGE_LOOP('',(#3201,#3202,#3203,#3204));
#896=EDGE_LOOP('',(#3205,#3206,#3207,#3208));
#897=EDGE_LOOP('',(#3209,#3210));
#898=EDGE_LOOP('',(#3211));
#899=EDGE_LOOP('',(#3212));
#900=EDGE_LOOP('',(#3213,#3214,#3215,#3216));
#901=EDGE_LOOP('',(#3217));
#902=EDGE_LOOP('',(#3218));
#903=EDGE_LOOP('',(#3219,#3220,#3221,#3222));
#904=EDGE_LOOP('',(#3223));
#905=EDGE_LOOP('',(#3224));
#906=EDGE_LOOP('',(#3225));
#907=EDGE_LOOP('',(#3226));
#908=EDGE_LOOP('',(#3227,#3228,#3229,#3230));
#909=EDGE_LOOP('',(#3231,#3232,#3233,#3234));
#910=EDGE_LOOP('',(#3235,#3236));
#911=EDGE_LOOP('',(#3237));
#912=EDGE_LOOP('',(#3238));
#913=EDGE_LOOP('',(#3239,#3240,#3241,#3242));
#914=EDGE_LOOP('',(#3243));
#915=EDGE_LOOP('',(#3244));
#916=EDGE_LOOP('',(#3245,#3246,#3247,#3248));
#917=EDGE_LOOP('',(#3249));
#918=EDGE_LOOP('',(#3250));
#919=EDGE_LOOP('',(#3251));
#920=EDGE_LOOP('',(#3252));
#921=EDGE_LOOP('',(#3253,#3254,#3255,#3256));
#922=EDGE_LOOP('',(#3257,#3258,#3259,#3260));
#923=EDGE_LOOP('',(#3261,#3262,#3263,#3264));
#924=EDGE_LOOP('',(#3265,#3266,#3267,#3268));
#925=EDGE_LOOP('',(#3269,#3270,#3271,#3272));
#926=EDGE_LOOP('',(#3273,#3274,#3275,#3276));
#927=EDGE_LOOP('',(#3277,#3278,#3279,#3280));
#928=EDGE_LOOP('',(#3281,#3282,#3283,#3284));
#929=EDGE_LOOP('',(#3285,#3286,#3287,#3288));
#930=EDGE_LOOP('',(#3289,#3290,#3291,#3292));
#931=EDGE_LOOP('',(#3293,#3294,#3295,#3296));
#932=EDGE_LOOP('',(#3297,#3298,#3299,#3300));
#933=EDGE_LOOP('',(#3301,#3302,#3303,#3304));
#934=EDGE_LOOP('',(#3305,#3306,#3307,#3308));
#935=EDGE_LOOP('',(#3309,#3310,#3311,#3312));
#936=EDGE_LOOP('',(#3313,#3314,#3315,#3316));
#937=EDGE_LOOP('',(#3317,#3318,#3319,#3320));
#938=EDGE_LOOP('',(#3321,#3322,#3323,#3324));
#939=EDGE_LOOP('',(#3325,#3326,#3327,#3328));
#940=EDGE_LOOP('',(#3329,#3330,#3331,#3332));
#941=EDGE_LOOP('',(#3333,#3334,#3335,#3336));
#942=EDGE_LOOP('',(#3337,#3338,#3339,#3340));
#943=EDGE_LOOP('',(#3341,#3342,#3343,#3344));
#944=EDGE_LOOP('',(#3345,#3346,#3347,#3348));
#945=EDGE_LOOP('',(#3349,#3350,#3351,#3352));
#946=EDGE_LOOP('',(#3353,#3354,#3355,#3356));
#947=EDGE_LOOP('',(#3357,#3358,#3359,#3360));
#948=EDGE_LOOP('',(#3361,#3362,#3363,#3364));
#949=EDGE_LOOP('',(#3365,#3366,#3367,#3368));
#950=EDGE_LOOP('',(#3369,#3370,#3371,#3372));
#951=EDGE_LOOP('',(#3373,#3374,#3375,#3376));
#952=EDGE_LOOP('',(#3377,#3378,#3379,#3380));
#953=EDGE_LOOP('',(#3381,#3382,#3383,#3384));
#954=EDGE_LOOP('',(#3385,#3386,#3387,#3388));
#955=EDGE_LOOP('',(#3389,#3390,#3391,#3392));
#956=EDGE_LOOP('',(#3393,#3394,#3395,#3396));
#957=EDGE_LOOP('',(#3397,#3398,#3399,#3400));
#958=EDGE_LOOP('',(#3401,#3402,#3403,#3404));
#959=EDGE_LOOP('',(#3405,#3406,#3407,#3408));
#960=EDGE_LOOP('',(#3409,#3410,#3411,#3412));
#961=EDGE_LOOP('',(#3413,#3414,#3415,#3416));
#962=EDGE_LOOP('',(#3417,#3418,#3419,#3420));
#963=EDGE_LOOP('',(#3421,#3422,#3423,#3424));
#964=EDGE_LOOP('',(#3425,#3426,#3427,#3428));
#965=EDGE_LOOP('',(#3429,#3430,#3431,#3432));
#966=EDGE_LOOP('',(#3433,#3434,#3435,#3436,#3437,#3438,#3439,#3440,#3441,
#3442,#3443,#3444,#3445,#3446,#3447,#3448,#3449,#3450,#3451,#3452,#3453,
#3454,#3455,#3456,#3457,#3458,#3459,#3460,#3461,#3462,#3463,#3464,#3465,
#3466,#3467,#3468,#3469,#3470,#3471,#3472,#3473,#3474,#3475,#3476));
#967=EDGE_LOOP('',(#3477));
#968=EDGE_LOOP('',(#3478,#3479,#3480,#3481,#3482,#3483,#3484,#3485,#3486,
#3487,#3488,#3489,#3490,#3491,#3492,#3493,#3494,#3495,#3496,#3497,#3498,
#3499,#3500,#3501,#3502,#3503,#3504,#3505,#3506,#3507,#3508,#3509,#3510,
#3511,#3512,#3513,#3514,#3515,#3516,#3517,#3518,#3519,#3520,#3521));
#969=EDGE_LOOP('',(#3522));
#970=EDGE_LOOP('',(#3523,#3524,#3525,#3526));
#971=EDGE_LOOP('',(#3527,#3528,#3529,#3530));
#972=EDGE_LOOP('',(#3531));
#973=EDGE_LOOP('',(#3532));
#974=EDGE_LOOP('',(#3533,#3534,#3535,#3536));
#975=EDGE_LOOP('',(#3537));
#976=EDGE_LOOP('',(#3538));
#977=EDGE_LOOP('',(#3539,#3540,#3541,#3542));
#978=EDGE_LOOP('',(#3543,#3544,#3545,#3546));
#979=EDGE_LOOP('',(#3547,#3548,#3549,#3550));
#980=EDGE_LOOP('',(#3551,#3552,#3553,#3554));
#981=EDGE_LOOP('',(#3555,#3556,#3557,#3558));
#982=EDGE_LOOP('',(#3559,#3560,#3561,#3562));
#983=EDGE_LOOP('',(#3563,#3564,#3565,#3566,#3567,#3568));
#984=EDGE_LOOP('',(#3569,#3570,#3571,#3572,#3573,#3574));
#985=EDGE_LOOP('',(#3575));
#986=EDGE_LOOP('',(#3576));
#987=EDGE_LOOP('',(#3577,#3578,#3579,#3580));
#988=EDGE_LOOP('',(#3581,#3582,#3583,#3584));
#989=EDGE_LOOP('',(#3585,#3586,#3587,#3588));
#990=EDGE_LOOP('',(#3589));
#991=EDGE_LOOP('',(#3590));
#992=EDGE_LOOP('',(#3591,#3592,#3593,#3594));
#993=EDGE_LOOP('',(#3595,#3596,#3597,#3598));
#994=EDGE_LOOP('',(#3599));
#995=EDGE_LOOP('',(#3600,#3601,#3602,#3603));
#996=EDGE_LOOP('',(#3604,#3605,#3606,#3607));
#997=EDGE_LOOP('',(#3608,#3609,#3610,#3611));
#998=EDGE_LOOP('',(#3612));
#999=EDGE_LOOP('',(#3613));
#1000=EDGE_LOOP('',(#3614,#3615,#3616,#3617));
#1001=EDGE_LOOP('',(#3618,#3619,#3620,#3621));
#1002=EDGE_LOOP('',(#3622,#3623,#3624,#3625));
#1003=EDGE_LOOP('',(#3626));
#1004=EDGE_LOOP('',(#3627,#3628,#3629,#3630));
#1005=EDGE_LOOP('',(#3631,#3632,#3633,#3634));
#1006=EDGE_LOOP('',(#3635,#3636,#3637,#3638));
#1007=EDGE_LOOP('',(#3639,#3640,#3641,#3642));
#1008=EDGE_LOOP('',(#3643,#3644,#3645,#3646));
#1009=EDGE_LOOP('',(#3647,#3648,#3649,#3650));
#1010=EDGE_LOOP('',(#3651,#3652,#3653,#3654,#3655,#3656));
#1011=EDGE_LOOP('',(#3657,#3658,#3659,#3660,#3661,#3662));
#1012=EDGE_LOOP('',(#3663,#3664,#3665,#3666,#3667,#3668));
#1013=EDGE_LOOP('',(#3669));
#1014=EDGE_LOOP('',(#3670,#3671,#3672,#3673,#3674,#3675));
#1015=EDGE_LOOP('',(#3676));
#1016=EDGE_LOOP('',(#3677,#3678,#3679,#3680));
#1017=EDGE_LOOP('',(#3681,#3682,#3683,#3684));
#1018=EDGE_LOOP('',(#3685,#3686,#3687,#3688));
#1019=EDGE_LOOP('',(#3689,#3690,#3691,#3692));
#1020=EDGE_LOOP('',(#3693,#3694,#3695,#3696));
#1021=EDGE_LOOP('',(#3697,#3698,#3699,#3700));
#1022=EDGE_LOOP('',(#3701,#3702,#3703,#3704));
#1023=EDGE_LOOP('',(#3705));
#1024=EDGE_LOOP('',(#3706));
#1025=EDGE_LOOP('',(#3707,#3708,#3709,#3710));
#1026=EDGE_LOOP('',(#3711,#3712,#3713,#3714));
#1027=EDGE_LOOP('',(#3715,#3716,#3717,#3718));
#1028=EDGE_LOOP('',(#3719));
#1029=EDGE_LOOP('',(#3720));
#1030=EDGE_LOOP('',(#3721,#3722,#3723,#3724));
#1031=EDGE_LOOP('',(#3725,#3726,#3727,#3728));
#1032=EDGE_LOOP('',(#3729));
#1033=EDGE_LOOP('',(#3730));
#1034=EDGE_LOOP('',(#3731,#3732,#3733,#3734));
#1035=EDGE_LOOP('',(#3735,#3736,#3737,#3738));
#1036=EDGE_LOOP('',(#3739));
#1037=EDGE_LOOP('',(#3740));
#1038=EDGE_LOOP('',(#3741,#3742));
#1039=EDGE_LOOP('',(#3743));
#1040=EDGE_LOOP('',(#3744));
#1041=EDGE_LOOP('',(#3745,#3746,#3747,#3748));
#1042=EDGE_LOOP('',(#3749,#3750,#3751,#3752));
#1043=EDGE_LOOP('',(#3753));
#1044=EDGE_LOOP('',(#3754));
#1045=EDGE_LOOP('',(#3755));
#1046=EDGE_LOOP('',(#3756));
#1047=EDGE_LOOP('',(#3757,#3758,#3759,#3760));
#1048=EDGE_LOOP('',(#3761));
#1049=EDGE_LOOP('',(#3762));
#1050=EDGE_LOOP('',(#3763,#3764,#3765,#3766));
#1051=EDGE_LOOP('',(#3767,#3768,#3769,#3770));
#1052=EDGE_LOOP('',(#3771));
#1053=EDGE_LOOP('',(#3772));
#1054=EDGE_LOOP('',(#3773));
#1055=EDGE_LOOP('',(#3774));
#1056=EDGE_LOOP('',(#3775,#3776,#3777,#3778));
#1057=EDGE_LOOP('',(#3779));
#1058=EDGE_LOOP('',(#3780));
#1059=EDGE_LOOP('',(#3781,#3782,#3783,#3784));
#1060=EDGE_LOOP('',(#3785,#3786,#3787,#3788));
#1061=EDGE_LOOP('',(#3789));
#1062=EDGE_LOOP('',(#3790));
#1063=EDGE_LOOP('',(#3791,#3792));
#1064=EDGE_LOOP('',(#3793));
#1065=EDGE_LOOP('',(#3794));
#1066=EDGE_LOOP('',(#3795,#3796,#3797,#3798));
#1067=EDGE_LOOP('',(#3799,#3800,#3801,#3802));
#1068=EDGE_LOOP('',(#3803));
#1069=EDGE_LOOP('',(#3804));
#1070=EDGE_LOOP('',(#3805));
#1071=EDGE_LOOP('',(#3806));
#1072=EDGE_LOOP('',(#3807,#3808,#3809,#3810));
#1073=EDGE_LOOP('',(#3811));
#1074=EDGE_LOOP('',(#3812));
#1075=EDGE_LOOP('',(#3813,#3814,#3815,#3816));
#1076=EDGE_LOOP('',(#3817,#3818,#3819,#3820));
#1077=EDGE_LOOP('',(#3821));
#1078=EDGE_LOOP('',(#3822));
#1079=EDGE_LOOP('',(#3823));
#1080=EDGE_LOOP('',(#3824));
#1081=EDGE_LOOP('',(#3825,#3826,#3827,#3828));
#1082=EDGE_LOOP('',(#3829));
#1083=EDGE_LOOP('',(#3830));
#1084=EDGE_LOOP('',(#3831,#3832,#3833,#3834));
#1085=EDGE_LOOP('',(#3835,#3836,#3837,#3838));
#1086=EDGE_LOOP('',(#3839));
#1087=EDGE_LOOP('',(#3840));
#1088=EDGE_LOOP('',(#3841,#3842));
#1089=EDGE_LOOP('',(#3843));
#1090=EDGE_LOOP('',(#3844));
#1091=EDGE_LOOP('',(#3845,#3846,#3847,#3848));
#1092=EDGE_LOOP('',(#3849,#3850,#3851,#3852));
#1093=EDGE_LOOP('',(#3853));
#1094=EDGE_LOOP('',(#3854));
#1095=EDGE_LOOP('',(#3855));
#1096=EDGE_LOOP('',(#3856));
#1097=EDGE_LOOP('',(#3857,#3858,#3859,#3860));
#1098=EDGE_LOOP('',(#3861));
#1099=EDGE_LOOP('',(#3862));
#1100=EDGE_LOOP('',(#3863,#3864,#3865,#3866));
#1101=EDGE_LOOP('',(#3867,#3868,#3869,#3870));
#1102=EDGE_LOOP('',(#3871));
#1103=EDGE_LOOP('',(#3872));
#1104=EDGE_LOOP('',(#3873));
#1105=EDGE_LOOP('',(#3874));
#1106=EDGE_LOOP('',(#3875,#3876,#3877,#3878));
#1107=EDGE_LOOP('',(#3879));
#1108=EDGE_LOOP('',(#3880));
#1109=EDGE_LOOP('',(#3881,#3882,#3883,#3884,#3885,#3886));
#1110=EDGE_LOOP('',(#3887));
#1111=EDGE_LOOP('',(#3888,#3889,#3890,#3891,#3892,#3893));
#1112=EDGE_LOOP('',(#3894));
#1113=EDGE_LOOP('',(#3895,#3896,#3897,#3898));
#1114=EDGE_LOOP('',(#3899,#3900,#3901,#3902));
#1115=EDGE_LOOP('',(#3903,#3904,#3905,#3906));
#1116=EDGE_LOOP('',(#3907,#3908,#3909,#3910));
#1117=EDGE_LOOP('',(#3911,#3912,#3913,#3914));
#1118=EDGE_LOOP('',(#3915,#3916,#3917,#3918));
#1119=EDGE_LOOP('',(#3919));
#1120=EDGE_LOOP('',(#3920));
#1121=EDGE_LOOP('',(#3921,#3922,#3923,#3924));
#1122=EDGE_LOOP('',(#3925));
#1123=EDGE_LOOP('',(#3926));
#1124=EDGE_LOOP('',(#3927,#3928,#3929,#3930));
#1125=EDGE_LOOP('',(#3931,#3932,#3933,#3934));
#1126=EDGE_LOOP('',(#3935));
#1127=EDGE_LOOP('',(#3936));
#1128=EDGE_LOOP('',(#3937,#3938,#3939,#3940));
#1129=EDGE_LOOP('',(#3941));
#1130=EDGE_LOOP('',(#3942));
#1131=EDGE_LOOP('',(#3943,#3944,#3945,#3946));
#1132=EDGE_LOOP('',(#3947));
#1133=EDGE_LOOP('',(#3948));
#1134=EDGE_LOOP('',(#3949,#3950,#3951,#3952));
#1135=EDGE_LOOP('',(#3953));
#1136=EDGE_LOOP('',(#3954));
#1137=EDGE_LOOP('',(#3955,#3956,#3957,#3958));
#1138=LINE('',#6399,#1492);
#1139=LINE('',#6404,#1493);
#1140=LINE('',#6406,#1494);
#1141=LINE('',#6408,#1495);
#1142=LINE('',#6409,#1496);
#1143=LINE('',#6412,#1497);
#1144=LINE('',#6414,#1498);
#1145=LINE('',#6415,#1499);
#1146=LINE('',#6418,#1500);
#1147=LINE('',#6420,#1501);
#1148=LINE('',#6421,#1502);
#1149=LINE('',#6423,#1503);
#1150=LINE('',#6424,#1504);
#1151=LINE('',#6431,#1505);
#1152=LINE('',#6433,#1506);
#1153=LINE('',#6435,#1507);
#1154=LINE('',#6436,#1508);
#1155=LINE('',#6439,#1509);
#1156=LINE('',#6441,#1510);
#1157=LINE('',#6442,#1511);
#1158=LINE('',#6445,#1512);
#1159=LINE('',#6447,#1513);
#1160=LINE('',#6448,#1514);
#1161=LINE('',#6450,#1515);
#1162=LINE('',#6451,#1516);
#1163=LINE('',#6458,#1517);
#1164=LINE('',#6460,#1518);
#1165=LINE('',#6462,#1519);
#1166=LINE('',#6463,#1520);
#1167=LINE('',#6466,#1521);
#1168=LINE('',#6468,#1522);
#1169=LINE('',#6469,#1523);
#1170=LINE('',#6472,#1524);
#1171=LINE('',#6474,#1525);
#1172=LINE('',#6475,#1526);
#1173=LINE('',#6477,#1527);
#1174=LINE('',#6478,#1528);
#1175=LINE('',#6486,#1529);
#1176=LINE('',#6492,#1530);
#1177=LINE('',#6498,#1531);
#1178=LINE('',#6503,#1532);
#1179=LINE('',#6505,#1533);
#1180=LINE('',#6507,#1534);
#1181=LINE('',#6508,#1535);
#1182=LINE('',#6511,#1536);
#1183=LINE('',#6513,#1537);
#1184=LINE('',#6514,#1538);
#1185=LINE('',#6517,#1539);
#1186=LINE('',#6519,#1540);
#1187=LINE('',#6520,#1541);
#1188=LINE('',#6522,#1542);
#1189=LINE('',#6523,#1543);
#1190=LINE('',#6530,#1544);
#1191=LINE('',#6536,#1545);
#1192=LINE('',#6611,#1546);
#1193=LINE('',#6616,#1547);
#1194=LINE('',#6622,#1548);
#1195=LINE('',#6628,#1549);
#1196=LINE('',#6703,#1550);
#1197=LINE('',#6708,#1551);
#1198=LINE('',#6714,#1552);
#1199=LINE('',#6720,#1553);
#1200=LINE('',#6795,#1554);
#1201=LINE('',#6800,#1555);
#1202=LINE('',#6807,#1556);
#1203=LINE('',#6858,#1557);
#1204=LINE('',#6859,#1558);
#1205=LINE('',#6860,#1559);
#1206=LINE('',#6861,#1560);
#1207=LINE('',#6866,#1561);
#1208=LINE('',#6875,#1562);
#1209=LINE('',#6883,#1563);
#1210=LINE('',#6887,#1564);
#1211=LINE('',#6891,#1565);
#1212=LINE('',#6893,#1566);
#1213=LINE('',#6895,#1567);
#1214=LINE('',#6896,#1568);
#1215=LINE('',#6899,#1569);
#1216=LINE('',#6901,#1570);
#1217=LINE('',#6902,#1571);
#1218=LINE('',#6905,#1572);
#1219=LINE('',#6907,#1573);
#1220=LINE('',#6908,#1574);
#1221=LINE('',#6910,#1575);
#1222=LINE('',#6911,#1576);
#1223=LINE('',#6919,#1577);
#1224=LINE('',#6928,#1578);
#1225=LINE('',#6934,#1579);
#1226=LINE('',#6944,#1580);
#1227=LINE('',#6951,#1581);
#1228=LINE('',#6960,#1582);
#1229=LINE('',#6966,#1583);
#1230=LINE('',#6976,#1584);
#1231=LINE('',#6983,#1585);
#1232=LINE('',#6992,#1586);
#1233=LINE('',#6998,#1587);
#1234=LINE('',#7008,#1588);
#1235=LINE('',#7015,#1589);
#1236=LINE('',#7023,#1590);
#1237=LINE('',#7025,#1591);
#1238=LINE('',#7027,#1592);
#1239=LINE('',#7028,#1593);
#1240=LINE('',#7031,#1594);
#1241=LINE('',#7033,#1595);
#1242=LINE('',#7034,#1596);
#1243=LINE('',#7037,#1597);
#1244=LINE('',#7039,#1598);
#1245=LINE('',#7040,#1599);
#1246=LINE('',#7043,#1600);
#1247=LINE('',#7045,#1601);
#1248=LINE('',#7046,#1602);
#1249=LINE('',#7049,#1603);
#1250=LINE('',#7051,#1604);
#1251=LINE('',#7052,#1605);
#1252=LINE('',#7055,#1606);
#1253=LINE('',#7057,#1607);
#1254=LINE('',#7058,#1608);
#1255=LINE('',#7061,#1609);
#1256=LINE('',#7063,#1610);
#1257=LINE('',#7064,#1611);
#1258=LINE('',#7067,#1612);
#1259=LINE('',#7069,#1613);
#1260=LINE('',#7070,#1614);
#1261=LINE('',#7073,#1615);
#1262=LINE('',#7075,#1616);
#1263=LINE('',#7076,#1617);
#1264=LINE('',#7080,#1618);
#1265=LINE('',#7082,#1619);
#1266=LINE('',#7084,#1620);
#1267=LINE('',#7085,#1621);
#1268=LINE('',#7088,#1622);
#1269=LINE('',#7090,#1623);
#1270=LINE('',#7091,#1624);
#1271=LINE('',#7094,#1625);
#1272=LINE('',#7096,#1626);
#1273=LINE('',#7097,#1627);
#1274=LINE('',#7100,#1628);
#1275=LINE('',#7102,#1629);
#1276=LINE('',#7103,#1630);
#1277=LINE('',#7106,#1631);
#1278=LINE('',#7108,#1632);
#1279=LINE('',#7109,#1633);
#1280=LINE('',#7112,#1634);
#1281=LINE('',#7114,#1635);
#1282=LINE('',#7115,#1636);
#1283=LINE('',#7118,#1637);
#1284=LINE('',#7120,#1638);
#1285=LINE('',#7121,#1639);
#1286=LINE('',#7124,#1640);
#1287=LINE('',#7126,#1641);
#1288=LINE('',#7127,#1642);
#1289=LINE('',#7130,#1643);
#1290=LINE('',#7132,#1644);
#1291=LINE('',#7133,#1645);
#1292=LINE('',#7137,#1646);
#1293=LINE('',#7139,#1647);
#1294=LINE('',#7141,#1648);
#1295=LINE('',#7142,#1649);
#1296=LINE('',#7145,#1650);
#1297=LINE('',#7147,#1651);
#1298=LINE('',#7148,#1652);
#1299=LINE('',#7151,#1653);
#1300=LINE('',#7153,#1654);
#1301=LINE('',#7154,#1655);
#1302=LINE('',#7157,#1656);
#1303=LINE('',#7159,#1657);
#1304=LINE('',#7160,#1658);
#1305=LINE('',#7163,#1659);
#1306=LINE('',#7165,#1660);
#1307=LINE('',#7166,#1661);
#1308=LINE('',#7169,#1662);
#1309=LINE('',#7171,#1663);
#1310=LINE('',#7172,#1664);
#1311=LINE('',#7175,#1665);
#1312=LINE('',#7177,#1666);
#1313=LINE('',#7178,#1667);
#1314=LINE('',#7181,#1668);
#1315=LINE('',#7183,#1669);
#1316=LINE('',#7184,#1670);
#1317=LINE('',#7187,#1671);
#1318=LINE('',#7189,#1672);
#1319=LINE('',#7190,#1673);
#1320=LINE('',#7194,#1674);
#1321=LINE('',#7196,#1675);
#1322=LINE('',#7198,#1676);
#1323=LINE('',#7199,#1677);
#1324=LINE('',#7202,#1678);
#1325=LINE('',#7204,#1679);
#1326=LINE('',#7205,#1680);
#1327=LINE('',#7208,#1681);
#1328=LINE('',#7210,#1682);
#1329=LINE('',#7211,#1683);
#1330=LINE('',#7214,#1684);
#1331=LINE('',#7216,#1685);
#1332=LINE('',#7217,#1686);
#1333=LINE('',#7220,#1687);
#1334=LINE('',#7222,#1688);
#1335=LINE('',#7223,#1689);
#1336=LINE('',#7226,#1690);
#1337=LINE('',#7228,#1691);
#1338=LINE('',#7229,#1692);
#1339=LINE('',#7232,#1693);
#1340=LINE('',#7234,#1694);
#1341=LINE('',#7235,#1695);
#1342=LINE('',#7238,#1696);
#1343=LINE('',#7240,#1697);
#1344=LINE('',#7241,#1698);
#1345=LINE('',#7244,#1699);
#1346=LINE('',#7246,#1700);
#1347=LINE('',#7247,#1701);
#1348=LINE('',#7252,#1702);
#1349=LINE('',#7256,#1703);
#1350=LINE('',#7258,#1704);
#1351=LINE('',#7259,#1705);
#1352=LINE('',#7262,#1706);
#1353=LINE('',#7264,#1707);
#1354=LINE('',#7265,#1708);
#1355=LINE('',#7267,#1709);
#1356=LINE('',#7268,#1710);
#1357=LINE('',#7271,#1711);
#1358=LINE('',#7273,#1712);
#1359=LINE('',#7274,#1713);
#1360=LINE('',#7276,#1714);
#1361=LINE('',#7277,#1715);
#1362=LINE('',#7280,#1716);
#1363=LINE('',#7282,#1717);
#1364=LINE('',#7283,#1718);
#1365=LINE('',#7285,#1719);
#1366=LINE('',#7286,#1720);
#1367=LINE('',#7288,#1721);
#1368=LINE('',#7289,#1722);
#1369=LINE('',#7297,#1723);
#1370=LINE('',#7301,#1724);
#1371=LINE('',#7308,#1725);
#1372=LINE('',#7315,#1726);
#1373=LINE('',#7317,#1727);
#1374=LINE('',#7319,#1728);
#1375=LINE('',#7320,#1729);
#1376=LINE('',#7323,#1730);
#1377=LINE('',#7325,#1731);
#1378=LINE('',#7326,#1732);
#1379=LINE('',#7329,#1733);
#1380=LINE('',#7331,#1734);
#1381=LINE('',#7332,#1735);
#1382=LINE('',#7335,#1736);
#1383=LINE('',#7337,#1737);
#1384=LINE('',#7338,#1738);
#1385=LINE('',#7341,#1739);
#1386=LINE('',#7343,#1740);
#1387=LINE('',#7344,#1741);
#1388=LINE('',#7346,#1742);
#1389=LINE('',#7347,#1743);
#1390=LINE('',#7359,#1744);
#1391=LINE('',#7363,#1745);
#1392=LINE('',#7367,#1746);
#1393=LINE('',#7374,#1747);
#1394=LINE('',#7376,#1748);
#1395=LINE('',#7384,#1749);
#1396=LINE('',#7388,#1750);
#1397=LINE('',#7392,#1751);
#1398=LINE('',#7399,#1752);
#1399=LINE('',#7403,#1753);
#1400=LINE('',#7407,#1754);
#1401=LINE('',#7412,#1755);
#1402=LINE('',#7414,#1756);
#1403=LINE('',#7416,#1757);
#1404=LINE('',#7417,#1758);
#1405=LINE('',#7420,#1759);
#1406=LINE('',#7422,#1760);
#1407=LINE('',#7423,#1761);
#1408=LINE('',#7426,#1762);
#1409=LINE('',#7428,#1763);
#1410=LINE('',#7429,#1764);
#1411=LINE('',#7432,#1765);
#1412=LINE('',#7434,#1766);
#1413=LINE('',#7435,#1767);
#1414=LINE('',#7438,#1768);
#1415=LINE('',#7440,#1769);
#1416=LINE('',#7441,#1770);
#1417=LINE('',#7443,#1771);
#1418=LINE('',#7444,#1772);
#1419=LINE('',#7451,#1773);
#1420=LINE('',#7453,#1774);
#1421=LINE('',#7455,#1775);
#1422=LINE('',#7457,#1776);
#1423=LINE('',#7459,#1777);
#1424=LINE('',#7460,#1778);
#1425=LINE('',#7466,#1779);
#1426=LINE('',#7468,#1780);
#1427=LINE('',#7470,#1781);
#1428=LINE('',#7472,#1782);
#1429=LINE('',#7474,#1783);
#1430=LINE('',#7475,#1784);
#1431=LINE('',#7479,#1785);
#1432=LINE('',#7480,#1786);
#1433=LINE('',#7482,#1787);
#1434=LINE('',#7484,#1788);
#1435=LINE('',#7486,#1789);
#1436=LINE('',#7488,#1790);
#1437=LINE('',#7492,#1791);
#1438=LINE('',#7500,#1792);
#1439=LINE('',#7504,#1793);
#1440=LINE('',#7508,#1794);
#1441=LINE('',#7513,#1795);
#1442=LINE('',#7537,#1796);
#1443=LINE('',#7544,#1797);
#1444=LINE('',#7550,#1798);
#1445=LINE('',#7562,#1799);
#1446=LINE('',#7568,#1800);
#1447=LINE('',#7577,#1801);
#1448=LINE('',#7584,#1802);
#1449=LINE('',#7590,#1803);
#1450=LINE('',#7600,#1804);
#1451=LINE('',#7607,#1805);
#1452=LINE('',#7613,#1806);
#1453=LINE('',#7625,#1807);
#1454=LINE('',#7631,#1808);
#1455=LINE('',#7640,#1809);
#1456=LINE('',#7647,#1810);
#1457=LINE('',#7653,#1811);
#1458=LINE('',#7663,#1812);
#1459=LINE('',#7670,#1813);
#1460=LINE('',#7676,#1814);
#1461=LINE('',#7688,#1815);
#1462=LINE('',#7694,#1816);
#1463=LINE('',#7703,#1817);
#1464=LINE('',#7710,#1818);
#1465=LINE('',#7716,#1819);
#1466=LINE('',#7726,#1820);
#1467=LINE('',#7734,#1821);
#1468=LINE('',#7736,#1822);
#1469=LINE('',#7738,#1823);
#1470=LINE('',#7740,#1824);
#1471=LINE('',#7742,#1825);
#1472=LINE('',#7743,#1826);
#1473=LINE('',#7749,#1827);
#1474=LINE('',#7751,#1828);
#1475=LINE('',#7753,#1829);
#1476=LINE('',#7755,#1830);
#1477=LINE('',#7757,#1831);
#1478=LINE('',#7758,#1832);
#1479=LINE('',#7762,#1833);
#1480=LINE('',#7763,#1834);
#1481=LINE('',#7765,#1835);
#1482=LINE('',#7767,#1836);
#1483=LINE('',#7769,#1837);
#1484=LINE('',#7771,#1838);
#1485=LINE('',#7778,#1839);
#1486=LINE('',#7784,#1840);
#1487=LINE('',#7788,#1841);
#1488=LINE('',#7793,#1842);
#1489=LINE('',#7803,#1843);
#1490=LINE('',#7810,#1844);
#1491=LINE('',#7815,#1845);
#1492=VECTOR('',#5082,0.275);
#1493=VECTOR('',#5087,1.);
#1494=VECTOR('',#5088,1.);
#1495=VECTOR('',#5089,1.);
#1496=VECTOR('',#5090,1.);
#1497=VECTOR('',#5093,1.);
#1498=VECTOR('',#5094,1.);
#1499=VECTOR('',#5095,1.);
#1500=VECTOR('',#5098,1.);
#1501=VECTOR('',#5099,1.);
#1502=VECTOR('',#5100,1.);
#1503=VECTOR('',#5103,1.);
#1504=VECTOR('',#5104,1.);
#1505=VECTOR('',#5113,1.);
#1506=VECTOR('',#5114,1.);
#1507=VECTOR('',#5115,1.);
#1508=VECTOR('',#5116,1.);
#1509=VECTOR('',#5119,1.);
#1510=VECTOR('',#5120,1.);
#1511=VECTOR('',#5121,1.);
#1512=VECTOR('',#5124,1.);
#1513=VECTOR('',#5125,1.);
#1514=VECTOR('',#5126,1.);
#1515=VECTOR('',#5129,1.);
#1516=VECTOR('',#5130,1.);
#1517=VECTOR('',#5139,1.);
#1518=VECTOR('',#5140,1.);
#1519=VECTOR('',#5141,1.);
#1520=VECTOR('',#5142,1.);
#1521=VECTOR('',#5145,1.);
#1522=VECTOR('',#5146,1.);
#1523=VECTOR('',#5147,1.);
#1524=VECTOR('',#5150,1.);
#1525=VECTOR('',#5151,1.);
#1526=VECTOR('',#5152,1.);
#1527=VECTOR('',#5155,1.);
#1528=VECTOR('',#5156,1.);
#1529=VECTOR('',#5167,0.165);
#1530=VECTOR('',#5174,0.165);
#1531=VECTOR('',#5181,0.275);
#1532=VECTOR('',#5186,1.);
#1533=VECTOR('',#5187,1.);
#1534=VECTOR('',#5188,1.);
#1535=VECTOR('',#5189,1.);
#1536=VECTOR('',#5192,1.);
#1537=VECTOR('',#5193,1.);
#1538=VECTOR('',#5194,1.);
#1539=VECTOR('',#5197,1.);
#1540=VECTOR('',#5198,1.);
#1541=VECTOR('',#5199,1.);
#1542=VECTOR('',#5202,1.);
#1543=VECTOR('',#5203,1.);
#1544=VECTOR('',#5212,1.);
#1545=VECTOR('',#5219,0.4);
#1546=VECTOR('',#5224,1.);
#1547=VECTOR('',#5229,1.2);
#1548=VECTOR('',#5236,1.);
#1549=VECTOR('',#5243,0.4);
#1550=VECTOR('',#5248,1.);
#1551=VECTOR('',#5253,1.2);
#1552=VECTOR('',#5260,1.);
#1553=VECTOR('',#5267,0.4);
#1554=VECTOR('',#5272,1.);
#1555=VECTOR('',#5277,1.2);
#1556=VECTOR('',#5286,0.684999999999999);
#1557=VECTOR('',#5297,0.300000000000001);
#1558=VECTOR('',#5298,0.300000000000001);
#1559=VECTOR('',#5299,0.300000000000001);
#1560=VECTOR('',#5300,0.300000000000001);
#1561=VECTOR('',#5305,0.4);
#1562=VECTOR('',#5316,0.4);
#1563=VECTOR('',#5327,0.225);
#1564=VECTOR('',#5332,0.225);
#1565=VECTOR('',#5335,1.);
#1566=VECTOR('',#5336,1.);
#1567=VECTOR('',#5337,1.);
#1568=VECTOR('',#5338,1.);
#1569=VECTOR('',#5341,1.);
#1570=VECTOR('',#5342,1.);
#1571=VECTOR('',#5343,1.);
#1572=VECTOR('',#5346,1.);
#1573=VECTOR('',#5347,1.);
#1574=VECTOR('',#5348,1.);
#1575=VECTOR('',#5351,1.);
#1576=VECTOR('',#5352,1.);
#1577=VECTOR('',#5363,0.300000000000001);
#1578=VECTOR('',#5376,0.4);
#1579=VECTOR('',#5383,0.85);
#1580=VECTOR('',#5394,1.2);
#1581=VECTOR('',#5403,1.4);
#1582=VECTOR('',#5416,0.4);
#1583=VECTOR('',#5423,0.85);
#1584=VECTOR('',#5434,1.2);
#1585=VECTOR('',#5443,1.4);
#1586=VECTOR('',#5456,0.4);
#1587=VECTOR('',#5463,0.85);
#1588=VECTOR('',#5474,1.2);
#1589=VECTOR('',#5483,1.4);
#1590=VECTOR('',#5494,1.);
#1591=VECTOR('',#5495,1.);
#1592=VECTOR('',#5496,1.);
#1593=VECTOR('',#5497,1.);
#1594=VECTOR('',#5500,1.);
#1595=VECTOR('',#5501,1.);
#1596=VECTOR('',#5502,1.);
#1597=VECTOR('',#5505,1.);
#1598=VECTOR('',#5506,1.);
#1599=VECTOR('',#5507,1.);
#1600=VECTOR('',#5510,1.);
#1601=VECTOR('',#5511,1.);
#1602=VECTOR('',#5512,1.);
#1603=VECTOR('',#5515,1.);
#1604=VECTOR('',#5516,1.);
#1605=VECTOR('',#5517,1.);
#1606=VECTOR('',#5520,1.);
#1607=VECTOR('',#5521,1.);
#1608=VECTOR('',#5522,1.);
#1609=VECTOR('',#5525,1.);
#1610=VECTOR('',#5526,1.);
#1611=VECTOR('',#5527,1.);
#1612=VECTOR('',#5530,1.);
#1613=VECTOR('',#5531,1.);
#1614=VECTOR('',#5532,1.);
#1615=VECTOR('',#5535,1.);
#1616=VECTOR('',#5536,1.);
#1617=VECTOR('',#5537,1.);
#1618=VECTOR('',#5540,1.);
#1619=VECTOR('',#5541,1.);
#1620=VECTOR('',#5542,1.);
#1621=VECTOR('',#5543,1.);
#1622=VECTOR('',#5546,1.);
#1623=VECTOR('',#5547,1.);
#1624=VECTOR('',#5548,1.);
#1625=VECTOR('',#5551,1.);
#1626=VECTOR('',#5552,1.);
#1627=VECTOR('',#5553,1.);
#1628=VECTOR('',#5556,1.);
#1629=VECTOR('',#5557,1.);
#1630=VECTOR('',#5558,1.);
#1631=VECTOR('',#5561,1.);
#1632=VECTOR('',#5562,1.);
#1633=VECTOR('',#5563,1.);
#1634=VECTOR('',#5566,1.);
#1635=VECTOR('',#5567,1.);
#1636=VECTOR('',#5568,1.);
#1637=VECTOR('',#5571,1.);
#1638=VECTOR('',#5572,1.);
#1639=VECTOR('',#5573,1.);
#1640=VECTOR('',#5576,1.);
#1641=VECTOR('',#5577,1.);
#1642=VECTOR('',#5578,1.);
#1643=VECTOR('',#5581,1.);
#1644=VECTOR('',#5582,1.);
#1645=VECTOR('',#5583,1.);
#1646=VECTOR('',#5586,1.);
#1647=VECTOR('',#5587,1.);
#1648=VECTOR('',#5588,1.);
#1649=VECTOR('',#5589,1.);
#1650=VECTOR('',#5592,1.);
#1651=VECTOR('',#5593,1.);
#1652=VECTOR('',#5594,1.);
#1653=VECTOR('',#5597,1.);
#1654=VECTOR('',#5598,1.);
#1655=VECTOR('',#5599,1.);
#1656=VECTOR('',#5602,1.);
#1657=VECTOR('',#5603,1.);
#1658=VECTOR('',#5604,1.);
#1659=VECTOR('',#5607,1.);
#1660=VECTOR('',#5608,1.);
#1661=VECTOR('',#5609,1.);
#1662=VECTOR('',#5612,1.);
#1663=VECTOR('',#5613,1.);
#1664=VECTOR('',#5614,1.);
#1665=VECTOR('',#5617,1.);
#1666=VECTOR('',#5618,1.);
#1667=VECTOR('',#5619,1.);
#1668=VECTOR('',#5622,1.);
#1669=VECTOR('',#5623,1.);
#1670=VECTOR('',#5624,1.);
#1671=VECTOR('',#5627,1.);
#1672=VECTOR('',#5628,1.);
#1673=VECTOR('',#5629,1.);
#1674=VECTOR('',#5632,1.);
#1675=VECTOR('',#5633,1.);
#1676=VECTOR('',#5634,1.);
#1677=VECTOR('',#5635,1.);
#1678=VECTOR('',#5638,1.);
#1679=VECTOR('',#5639,1.);
#1680=VECTOR('',#5640,1.);
#1681=VECTOR('',#5643,1.);
#1682=VECTOR('',#5644,1.);
#1683=VECTOR('',#5645,1.);
#1684=VECTOR('',#5648,1.);
#1685=VECTOR('',#5649,1.);
#1686=VECTOR('',#5650,1.);
#1687=VECTOR('',#5653,1.);
#1688=VECTOR('',#5654,1.);
#1689=VECTOR('',#5655,1.);
#1690=VECTOR('',#5658,1.);
#1691=VECTOR('',#5659,1.);
#1692=VECTOR('',#5660,1.);
#1693=VECTOR('',#5663,1.);
#1694=VECTOR('',#5664,1.);
#1695=VECTOR('',#5665,1.);
#1696=VECTOR('',#5668,1.);
#1697=VECTOR('',#5669,1.);
#1698=VECTOR('',#5670,1.);
#1699=VECTOR('',#5673,1.);
#1700=VECTOR('',#5674,1.);
#1701=VECTOR('',#5675,1.);
#1702=VECTOR('',#5680,0.21);
#1703=VECTOR('',#5685,1.);
#1704=VECTOR('',#5686,1.);
#1705=VECTOR('',#5687,1.);
#1706=VECTOR('',#5690,1.);
#1707=VECTOR('',#5691,1.);
#1708=VECTOR('',#5692,1.);
#1709=VECTOR('',#5695,1.);
#1710=VECTOR('',#5696,1.);
#1711=VECTOR('',#5699,1.);
#1712=VECTOR('',#5700,1.);
#1713=VECTOR('',#5701,1.);
#1714=VECTOR('',#5704,1.);
#1715=VECTOR('',#5705,1.);
#1716=VECTOR('',#5708,1.);
#1717=VECTOR('',#5709,1.);
#1718=VECTOR('',#5710,1.);
#1719=VECTOR('',#5713,1.);
#1720=VECTOR('',#5714,1.);
#1721=VECTOR('',#5717,1.);
#1722=VECTOR('',#5718,1.);
#1723=VECTOR('',#5729,0.275);
#1724=VECTOR('',#5734,0.265);
#1725=VECTOR('',#5743,0.5);
#1726=VECTOR('',#5752,1.);
#1727=VECTOR('',#5753,1.);
#1728=VECTOR('',#5754,1.);
#1729=VECTOR('',#5755,1.);
#1730=VECTOR('',#5758,1.);
#1731=VECTOR('',#5759,1.);
#1732=VECTOR('',#5760,1.);
#1733=VECTOR('',#5763,1.);
#1734=VECTOR('',#5764,1.);
#1735=VECTOR('',#5765,1.);
#1736=VECTOR('',#5768,1.);
#1737=VECTOR('',#5769,1.);
#1738=VECTOR('',#5770,1.);
#1739=VECTOR('',#5773,1.);
#1740=VECTOR('',#5774,1.);
#1741=VECTOR('',#5775,1.);
#1742=VECTOR('',#5778,1.);
#1743=VECTOR('',#5779,1.);
#1744=VECTOR('',#5796,0.4);
#1745=VECTOR('',#5801,0.425);
#1746=VECTOR('',#5806,0.41);
#1747=VECTOR('',#5815,0.26);
#1748=VECTOR('',#5818,0.25);
#1749=VECTOR('',#5829,0.325);
#1750=VECTOR('',#5834,0.35);
#1751=VECTOR('',#5839,0.335);
#1752=VECTOR('',#5848,0.21);
#1753=VECTOR('',#5853,0.2);
#1754=VECTOR('',#5858,0.18);
#1755=VECTOR('',#5863,1.);
#1756=VECTOR('',#5864,1.);
#1757=VECTOR('',#5865,1.);
#1758=VECTOR('',#5866,1.);
#1759=VECTOR('',#5869,1.);
#1760=VECTOR('',#5870,1.);
#1761=VECTOR('',#5871,1.);
#1762=VECTOR('',#5874,1.);
#1763=VECTOR('',#5875,1.);
#1764=VECTOR('',#5876,1.);
#1765=VECTOR('',#5879,1.);
#1766=VECTOR('',#5880,1.);
#1767=VECTOR('',#5881,1.);
#1768=VECTOR('',#5884,1.);
#1769=VECTOR('',#5885,1.);
#1770=VECTOR('',#5886,1.);
#1771=VECTOR('',#5889,1.);
#1772=VECTOR('',#5890,1.);
#1773=VECTOR('',#5899,1.);
#1774=VECTOR('',#5900,1.);
#1775=VECTOR('',#5901,1.);
#1776=VECTOR('',#5902,1.);
#1777=VECTOR('',#5903,1.);
#1778=VECTOR('',#5904,1.);
#1779=VECTOR('',#5909,1.);
#1780=VECTOR('',#5910,1.);
#1781=VECTOR('',#5911,1.);
#1782=VECTOR('',#5912,1.);
#1783=VECTOR('',#5913,1.);
#1784=VECTOR('',#5914,1.);
#1785=VECTOR('',#5919,1.);
#1786=VECTOR('',#5920,1.);
#1787=VECTOR('',#5923,1.);
#1788=VECTOR('',#5926,1.);
#1789=VECTOR('',#5929,1.);
#1790=VECTOR('',#5932,1.);
#1791=VECTOR('',#5937,0.685);
#1792=VECTOR('',#5948,0.645);
#1793=VECTOR('',#5953,0.685);
#1794=VECTOR('',#5958,0.645);
#1795=VECTOR('',#5965,0.46);
#1796=VECTOR('',#6008,0.515);
#1797=VECTOR('',#6017,0.2);
#1798=VECTOR('',#6024,0.6);
#1799=VECTOR('',#6039,0.2);
#1800=VECTOR('',#6046,0.3);
#1801=VECTOR('',#6059,0.3);
#1802=VECTOR('',#6068,0.0750000000000002);
#1803=VECTOR('',#6075,0.4);
#1804=VECTOR('',#6090,0.515);
#1805=VECTOR('',#6099,0.2);
#1806=VECTOR('',#6106,0.6);
#1807=VECTOR('',#6121,0.2);
#1808=VECTOR('',#6128,0.3);
#1809=VECTOR('',#6141,0.3);
#1810=VECTOR('',#6150,0.075);
#1811=VECTOR('',#6157,0.4);
#1812=VECTOR('',#6172,0.515);
#1813=VECTOR('',#6181,0.2);
#1814=VECTOR('',#6188,0.6);
#1815=VECTOR('',#6203,0.2);
#1816=VECTOR('',#6210,0.3);
#1817=VECTOR('',#6223,0.3);
#1818=VECTOR('',#6232,0.0750000000000002);
#1819=VECTOR('',#6239,0.4);
#1820=VECTOR('',#6254,0.43);
#1821=VECTOR('',#6263,1.);
#1822=VECTOR('',#6264,1.);
#1823=VECTOR('',#6265,1.);
#1824=VECTOR('',#6266,1.);
#1825=VECTOR('',#6267,1.);
#1826=VECTOR('',#6268,1.);
#1827=VECTOR('',#6273,1.);
#1828=VECTOR('',#6274,1.);
#1829=VECTOR('',#6275,1.);
#1830=VECTOR('',#6276,1.);
#1831=VECTOR('',#6277,1.);
#1832=VECTOR('',#6278,1.);
#1833=VECTOR('',#6283,1.);
#1834=VECTOR('',#6284,1.);
#1835=VECTOR('',#6287,1.);
#1836=VECTOR('',#6290,1.);
#1837=VECTOR('',#6293,1.);
#1838=VECTOR('',#6296,1.);
#1839=VECTOR('',#6305,0.46);
#1840=VECTOR('',#6314,0.525);
#1841=VECTOR('',#6319,0.515);
#1842=VECTOR('',#6326,0.2);
#1843=VECTOR('',#6339,0.475);
#1844=VECTOR('',#6348,0.355);
#1845=VECTOR('',#6355,0.31);
#1846=CIRCLE('',#4593,0.275);
#1847=CIRCLE('',#4594,0.275);
#1848=CIRCLE('',#4617,0.165);
#1849=CIRCLE('',#4618,0.165);
#1850=CIRCLE('',#4620,0.165);
#1851=CIRCLE('',#4621,0.165);
#1852=CIRCLE('',#4623,0.275);
#1853=CIRCLE('',#4624,0.275);
#1854=CIRCLE('',#4633,0.4);
#1855=CIRCLE('',#4635,0.4);
#1856=CIRCLE('',#4636,0.4);
#1857=CIRCLE('',#4639,1.2);
#1858=CIRCLE('',#4640,1.2);
#1859=CIRCLE('',#4643,0.4);
#1860=CIRCLE('',#4645,0.4);
#1861=CIRCLE('',#4646,0.4);
#1862=CIRCLE('',#4649,1.2);
#1863=CIRCLE('',#4650,1.2);
#1864=CIRCLE('',#4653,0.4);
#1865=CIRCLE('',#4655,0.4);
#1866=CIRCLE('',#4656,0.4);
#1867=CIRCLE('',#4659,1.2);
#1868=CIRCLE('',#4660,1.2);
#1869=CIRCLE('',#4663,0.684999999999999);
#1870=CIRCLE('',#4664,0.684999999999999);
#1871=CIRCLE('',#4666,0.300000000000001);
#1872=CIRCLE('',#4668,0.300000000000001);
#1873=CIRCLE('',#4670,0.4);
#1874=CIRCLE('',#4671,0.4);
#1875=CIRCLE('',#4673,0.225);
#1876=CIRCLE('',#4675,0.4);
#1877=CIRCLE('',#4676,0.4);
#1878=CIRCLE('',#4678,0.225);
#1879=CIRCLE('',#4680,0.225);
#1880=CIRCLE('',#4682,0.225);
#1881=CIRCLE('',#4691,0.300000000000001);
#1882=CIRCLE('',#4692,0.300000000000001);
#1883=CIRCLE('',#4697,0.4);
#1884=CIRCLE('',#4698,0.4);
#1885=CIRCLE('',#4700,0.85);
#1886=CIRCLE('',#4701,0.85);
#1887=CIRCLE('',#4703,1.);
#1888=CIRCLE('',#4705,1.2);
#1889=CIRCLE('',#4706,1.2);
#1890=CIRCLE('',#4709,1.4);
#1891=CIRCLE('',#4710,1.4);
#1892=CIRCLE('',#4715,0.4);
#1893=CIRCLE('',#4716,0.4);
#1894=CIRCLE('',#4718,0.85);
#1895=CIRCLE('',#4719,0.85);
#1896=CIRCLE('',#4721,1.);
#1897=CIRCLE('',#4723,1.2);
#1898=CIRCLE('',#4724,1.2);
#1899=CIRCLE('',#4727,1.4);
#1900=CIRCLE('',#4728,1.4);
#1901=CIRCLE('',#4733,0.4);
#1902=CIRCLE('',#4734,0.4);
#1903=CIRCLE('',#4736,0.85);
#1904=CIRCLE('',#4737,0.85);
#1905=CIRCLE('',#4739,1.);
#1906=CIRCLE('',#4741,1.2);
#1907=CIRCLE('',#4742,1.2);
#1908=CIRCLE('',#4745,1.4);
#1909=CIRCLE('',#4746,1.4);
#1910=CIRCLE('',#4787,0.21);
#1911=CIRCLE('',#4788,0.21);
#1912=CIRCLE('',#4801,0.285);
#1913=CIRCLE('',#4802,0.265);
#1914=CIRCLE('',#4804,0.265);
#1915=CIRCLE('',#4806,0.5);
#1916=CIRCLE('',#4808,0.5);
#1917=CIRCLE('',#4820,0.24505);
#1918=CIRCLE('',#4822,0.375);
#1919=CIRCLE('',#4824,0.425);
#1920=CIRCLE('',#4826,0.425);
#1921=CIRCLE('',#4828,0.395);
#1922=CIRCLE('',#4830,0.27);
#1923=CIRCLE('',#4832,0.24505);
#1924=CIRCLE('',#4836,0.3);
#1925=CIRCLE('',#4838,0.35);
#1926=CIRCLE('',#4840,0.35);
#1927=CIRCLE('',#4842,0.32);
#1928=CIRCLE('',#4844,0.22);
#1929=CIRCLE('',#4846,0.1954);
#1930=CIRCLE('',#4848,0.1954);
#1931=CIRCLE('',#4850,0.16);
#1932=CIRCLE('',#4862,0.685);
#1933=CIRCLE('',#4864,0.685);
#1934=CIRCLE('',#4872,0.685);
#1935=CIRCLE('',#4874,0.605);
#1936=CIRCLE('',#4875,0.46);
#1937=CIRCLE('',#4878,0.685);
#1938=CIRCLE('',#4880,0.605);
#1939=CIRCLE('',#4882,0.46);
#1940=CIRCLE('',#4904,0.515);
#1941=CIRCLE('',#4905,0.515);
#1942=CIRCLE('',#4907,0.2);
#1943=CIRCLE('',#4909,0.2);
#1944=CIRCLE('',#4911,0.6);
#1945=CIRCLE('',#4912,0.6);
#1946=CIRCLE('',#4915,1.);
#1947=CIRCLE('',#4918,0.2);
#1948=CIRCLE('',#4919,0.2);
#1949=CIRCLE('',#4921,0.3);
#1950=CIRCLE('',#4922,0.3);
#1951=CIRCLE('',#4927,0.3);
#1952=CIRCLE('',#4928,0.3);
#1953=CIRCLE('',#4930,0.0750000000000002);
#1954=CIRCLE('',#4932,0.0750000000000002);
#1955=CIRCLE('',#4934,0.4);
#1956=CIRCLE('',#4935,0.4);
#1957=CIRCLE('',#4941,0.515);
#1958=CIRCLE('',#4942,0.515);
#1959=CIRCLE('',#4944,0.2);
#1960=CIRCLE('',#4946,0.2);
#1961=CIRCLE('',#4948,0.6);
#1962=CIRCLE('',#4949,0.6);
#1963=CIRCLE('',#4952,1.);
#1964=CIRCLE('',#4955,0.2);
#1965=CIRCLE('',#4956,0.2);
#1966=CIRCLE('',#4958,0.3);
#1967=CIRCLE('',#4959,0.3);
#1968=CIRCLE('',#4964,0.3);
#1969=CIRCLE('',#4965,0.3);
#1970=CIRCLE('',#4967,0.075);
#1971=CIRCLE('',#4969,0.075);
#1972=CIRCLE('',#4971,0.4);
#1973=CIRCLE('',#4972,0.4);
#1974=CIRCLE('',#4978,0.515);
#1975=CIRCLE('',#4979,0.515);
#1976=CIRCLE('',#4981,0.2);
#1977=CIRCLE('',#4983,0.2);
#1978=CIRCLE('',#4985,0.6);
#1979=CIRCLE('',#4986,0.6);
#1980=CIRCLE('',#4989,1.);
#1981=CIRCLE('',#4992,0.2);
#1982=CIRCLE('',#4993,0.2);
#1983=CIRCLE('',#4995,0.3);
#1984=CIRCLE('',#4996,0.3);
#1985=CIRCLE('',#5001,0.3);
#1986=CIRCLE('',#5002,0.3);
#1987=CIRCLE('',#5004,0.0750000000000002);
#1988=CIRCLE('',#5006,0.0750000000000002);
#1989=CIRCLE('',#5008,0.4);
#1990=CIRCLE('',#5009,0.4);
#1991=CIRCLE('',#5015,0.43);
#1992=CIRCLE('',#5016,0.43);
#1993=CIRCLE('',#5018,0.2);
#1994=CIRCLE('',#5020,0.525);
#1995=CIRCLE('',#5022,0.515);
#1996=CIRCLE('',#5030,0.46);
#1997=CIRCLE('',#5032,0.46);
#1998=CIRCLE('',#5034,0.525);
#1999=CIRCLE('',#5037,0.515);
#2000=CIRCLE('',#5039,0.2);
#2001=CIRCLE('',#5043,0.475);
#2002=CIRCLE('',#5044,0.31);
#2003=CIRCLE('',#5046,0.475);
#2004=CIRCLE('',#5048,0.355);
#2005=CIRCLE('',#5050,0.355);
#2006=CIRCLE('',#5052,0.31);
#2007=VERTEX_POINT('',#6396);
#2008=VERTEX_POINT('',#6398);
#2009=VERTEX_POINT('',#6402);
#2010=VERTEX_POINT('',#6403);
#2011=VERTEX_POINT('',#6405);
#2012=VERTEX_POINT('',#6407);
#2013=VERTEX_POINT('',#6411);
#2014=VERTEX_POINT('',#6413);
#2015=VERTEX_POINT('',#6417);
#2016=VERTEX_POINT('',#6419);
#2017=VERTEX_POINT('',#6429);
#2018=VERTEX_POINT('',#6430);
#2019=VERTEX_POINT('',#6432);
#2020=VERTEX_POINT('',#6434);
#2021=VERTEX_POINT('',#6438);
#2022=VERTEX_POINT('',#6440);
#2023=VERTEX_POINT('',#6444);
#2024=VERTEX_POINT('',#6446);
#2025=VERTEX_POINT('',#6456);
#2026=VERTEX_POINT('',#6457);
#2027=VERTEX_POINT('',#6459);
#2028=VERTEX_POINT('',#6461);
#2029=VERTEX_POINT('',#6465);
#2030=VERTEX_POINT('',#6467);
#2031=VERTEX_POINT('',#6471);
#2032=VERTEX_POINT('',#6473);
#2033=VERTEX_POINT('',#6483);
#2034=VERTEX_POINT('',#6485);
#2035=VERTEX_POINT('',#6489);
#2036=VERTEX_POINT('',#6491);
#2037=VERTEX_POINT('',#6495);
#2038=VERTEX_POINT('',#6497);
#2039=VERTEX_POINT('',#6501);
#2040=VERTEX_POINT('',#6502);
#2041=VERTEX_POINT('',#6504);
#2042=VERTEX_POINT('',#6506);
#2043=VERTEX_POINT('',#6510);
#2044=VERTEX_POINT('',#6512);
#2045=VERTEX_POINT('',#6516);
#2046=VERTEX_POINT('',#6518);
#2047=VERTEX_POINT('',#6528);
#2048=VERTEX_POINT('',#6529);
#2049=VERTEX_POINT('',#6533);
#2050=VERTEX_POINT('',#6535);
#2051=VERTEX_POINT('',#6537);
#2052=VERTEX_POINT('',#6556);
#2053=VERTEX_POINT('',#6563);
#2054=VERTEX_POINT('',#6591);
#2055=VERTEX_POINT('',#6613);
#2056=VERTEX_POINT('',#6615);
#2057=VERTEX_POINT('',#6620);
#2058=VERTEX_POINT('',#6621);
#2059=VERTEX_POINT('',#6625);
#2060=VERTEX_POINT('',#6627);
#2061=VERTEX_POINT('',#6629);
#2062=VERTEX_POINT('',#6648);
#2063=VERTEX_POINT('',#6655);
#2064=VERTEX_POINT('',#6683);
#2065=VERTEX_POINT('',#6705);
#2066=VERTEX_POINT('',#6707);
#2067=VERTEX_POINT('',#6712);
#2068=VERTEX_POINT('',#6713);
#2069=VERTEX_POINT('',#6717);
#2070=VERTEX_POINT('',#6719);
#2071=VERTEX_POINT('',#6721);
#2072=VERTEX_POINT('',#6740);
#2073=VERTEX_POINT('',#6747);
#2074=VERTEX_POINT('',#6775);
#2075=VERTEX_POINT('',#6797);
#2076=VERTEX_POINT('',#6799);
#2077=VERTEX_POINT('',#6804);
#2078=VERTEX_POINT('',#6806);
#2079=VERTEX_POINT('',#6809);
#2080=VERTEX_POINT('',#6853);
#2081=VERTEX_POINT('',#6856);
#2082=VERTEX_POINT('',#6863);
#2083=VERTEX_POINT('',#6865);
#2084=VERTEX_POINT('',#6869);
#2085=VERTEX_POINT('',#6872);
#2086=VERTEX_POINT('',#6874);
#2087=VERTEX_POINT('',#6878);
#2088=VERTEX_POINT('',#6881);
#2089=VERTEX_POINT('',#6885);
#2090=VERTEX_POINT('',#6889);
#2091=VERTEX_POINT('',#6890);
#2092=VERTEX_POINT('',#6892);
#2093=VERTEX_POINT('',#6894);
#2094=VERTEX_POINT('',#6898);
#2095=VERTEX_POINT('',#6900);
#2096=VERTEX_POINT('',#6904);
#2097=VERTEX_POINT('',#6906);
#2098=VERTEX_POINT('',#6916);
#2099=VERTEX_POINT('',#6918);
#2100=VERTEX_POINT('',#6925);
#2101=VERTEX_POINT('',#6927);
#2102=VERTEX_POINT('',#6931);
#2103=VERTEX_POINT('',#6933);
#2104=VERTEX_POINT('',#6937);
#2105=VERTEX_POINT('',#6938);
#2106=VERTEX_POINT('',#6941);
#2107=VERTEX_POINT('',#6943);
#2108=VERTEX_POINT('',#6948);
#2109=VERTEX_POINT('',#6950);
#2110=VERTEX_POINT('',#6957);
#2111=VERTEX_POINT('',#6959);
#2112=VERTEX_POINT('',#6963);
#2113=VERTEX_POINT('',#6965);
#2114=VERTEX_POINT('',#6969);
#2115=VERTEX_POINT('',#6970);
#2116=VERTEX_POINT('',#6973);
#2117=VERTEX_POINT('',#6975);
#2118=VERTEX_POINT('',#6980);
#2119=VERTEX_POINT('',#6982);
#2120=VERTEX_POINT('',#6989);
#2121=VERTEX_POINT('',#6991);
#2122=VERTEX_POINT('',#6995);
#2123=VERTEX_POINT('',#6997);
#2124=VERTEX_POINT('',#7001);
#2125=VERTEX_POINT('',#7002);
#2126=VERTEX_POINT('',#7005);
#2127=VERTEX_POINT('',#7007);
#2128=VERTEX_POINT('',#7012);
#2129=VERTEX_POINT('',#7014);
#2130=VERTEX_POINT('',#7021);
#2131=VERTEX_POINT('',#7022);
#2132=VERTEX_POINT('',#7024);
#2133=VERTEX_POINT('',#7026);
#2134=VERTEX_POINT('',#7030);
#2135=VERTEX_POINT('',#7032);
#2136=VERTEX_POINT('',#7036);
#2137=VERTEX_POINT('',#7038);
#2138=VERTEX_POINT('',#7042);
#2139=VERTEX_POINT('',#7044);
#2140=VERTEX_POINT('',#7048);
#2141=VERTEX_POINT('',#7050);
#2142=VERTEX_POINT('',#7054);
#2143=VERTEX_POINT('',#7056);
#2144=VERTEX_POINT('',#7060);
#2145=VERTEX_POINT('',#7062);
#2146=VERTEX_POINT('',#7066);
#2147=VERTEX_POINT('',#7068);
#2148=VERTEX_POINT('',#7072);
#2149=VERTEX_POINT('',#7074);
#2150=VERTEX_POINT('',#7078);
#2151=VERTEX_POINT('',#7079);
#2152=VERTEX_POINT('',#7081);
#2153=VERTEX_POINT('',#7083);
#2154=VERTEX_POINT('',#7087);
#2155=VERTEX_POINT('',#7089);
#2156=VERTEX_POINT('',#7093);
#2157=VERTEX_POINT('',#7095);
#2158=VERTEX_POINT('',#7099);
#2159=VERTEX_POINT('',#7101);
#2160=VERTEX_POINT('',#7105);
#2161=VERTEX_POINT('',#7107);
#2162=VERTEX_POINT('',#7111);
#2163=VERTEX_POINT('',#7113);
#2164=VERTEX_POINT('',#7117);
#2165=VERTEX_POINT('',#7119);
#2166=VERTEX_POINT('',#7123);
#2167=VERTEX_POINT('',#7125);
#2168=VERTEX_POINT('',#7129);
#2169=VERTEX_POINT('',#7131);
#2170=VERTEX_POINT('',#7135);
#2171=VERTEX_POINT('',#7136);
#2172=VERTEX_POINT('',#7138);
#2173=VERTEX_POINT('',#7140);
#2174=VERTEX_POINT('',#7144);
#2175=VERTEX_POINT('',#7146);
#2176=VERTEX_POINT('',#7150);
#2177=VERTEX_POINT('',#7152);
#2178=VERTEX_POINT('',#7156);
#2179=VERTEX_POINT('',#7158);
#2180=VERTEX_POINT('',#7162);
#2181=VERTEX_POINT('',#7164);
#2182=VERTEX_POINT('',#7168);
#2183=VERTEX_POINT('',#7170);
#2184=VERTEX_POINT('',#7174);
#2185=VERTEX_POINT('',#7176);
#2186=VERTEX_POINT('',#7180);
#2187=VERTEX_POINT('',#7182);
#2188=VERTEX_POINT('',#7186);
#2189=VERTEX_POINT('',#7188);
#2190=VERTEX_POINT('',#7192);
#2191=VERTEX_POINT('',#7193);
#2192=VERTEX_POINT('',#7195);
#2193=VERTEX_POINT('',#7197);
#2194=VERTEX_POINT('',#7201);
#2195=VERTEX_POINT('',#7203);
#2196=VERTEX_POINT('',#7207);
#2197=VERTEX_POINT('',#7209);
#2198=VERTEX_POINT('',#7213);
#2199=VERTEX_POINT('',#7215);
#2200=VERTEX_POINT('',#7219);
#2201=VERTEX_POINT('',#7221);
#2202=VERTEX_POINT('',#7225);
#2203=VERTEX_POINT('',#7227);
#2204=VERTEX_POINT('',#7231);
#2205=VERTEX_POINT('',#7233);
#2206=VERTEX_POINT('',#7237);
#2207=VERTEX_POINT('',#7239);
#2208=VERTEX_POINT('',#7243);
#2209=VERTEX_POINT('',#7245);
#2210=VERTEX_POINT('',#7249);
#2211=VERTEX_POINT('',#7251);
#2212=VERTEX_POINT('',#7255);
#2213=VERTEX_POINT('',#7257);
#2214=VERTEX_POINT('',#7261);
#2215=VERTEX_POINT('',#7263);
#2216=VERTEX_POINT('',#7270);
#2217=VERTEX_POINT('',#7272);
#2218=VERTEX_POINT('',#7279);
#2219=VERTEX_POINT('',#7281);
#2220=VERTEX_POINT('',#7294);
#2221=VERTEX_POINT('',#7296);
#2222=VERTEX_POINT('',#7300);
#2223=VERTEX_POINT('',#7304);
#2224=VERTEX_POINT('',#7307);
#2225=VERTEX_POINT('',#7313);
#2226=VERTEX_POINT('',#7314);
#2227=VERTEX_POINT('',#7316);
#2228=VERTEX_POINT('',#7318);
#2229=VERTEX_POINT('',#7322);
#2230=VERTEX_POINT('',#7324);
#2231=VERTEX_POINT('',#7328);
#2232=VERTEX_POINT('',#7330);
#2233=VERTEX_POINT('',#7334);
#2234=VERTEX_POINT('',#7336);
#2235=VERTEX_POINT('',#7340);
#2236=VERTEX_POINT('',#7342);
#2237=VERTEX_POINT('',#7351);
#2238=VERTEX_POINT('',#7354);
#2239=VERTEX_POINT('',#7357);
#2240=VERTEX_POINT('',#7361);
#2241=VERTEX_POINT('',#7365);
#2242=VERTEX_POINT('',#7369);
#2243=VERTEX_POINT('',#7372);
#2244=VERTEX_POINT('',#7379);
#2245=VERTEX_POINT('',#7382);
#2246=VERTEX_POINT('',#7386);
#2247=VERTEX_POINT('',#7390);
#2248=VERTEX_POINT('',#7394);
#2249=VERTEX_POINT('',#7397);
#2250=VERTEX_POINT('',#7401);
#2251=VERTEX_POINT('',#7405);
#2252=VERTEX_POINT('',#7410);
#2253=VERTEX_POINT('',#7411);
#2254=VERTEX_POINT('',#7413);
#2255=VERTEX_POINT('',#7415);
#2256=VERTEX_POINT('',#7419);
#2257=VERTEX_POINT('',#7421);
#2258=VERTEX_POINT('',#7425);
#2259=VERTEX_POINT('',#7427);
#2260=VERTEX_POINT('',#7431);
#2261=VERTEX_POINT('',#7433);
#2262=VERTEX_POINT('',#7437);
#2263=VERTEX_POINT('',#7439);
#2264=VERTEX_POINT('',#7449);
#2265=VERTEX_POINT('',#7450);
#2266=VERTEX_POINT('',#7452);
#2267=VERTEX_POINT('',#7454);
#2268=VERTEX_POINT('',#7456);
#2269=VERTEX_POINT('',#7458);
#2270=VERTEX_POINT('',#7461);
#2271=VERTEX_POINT('',#7464);
#2272=VERTEX_POINT('',#7465);
#2273=VERTEX_POINT('',#7467);
#2274=VERTEX_POINT('',#7469);
#2275=VERTEX_POINT('',#7471);
#2276=VERTEX_POINT('',#7473);
#2277=VERTEX_POINT('',#7476);
#2278=VERTEX_POINT('',#7491);
#2279=VERTEX_POINT('',#7495);
#2280=VERTEX_POINT('',#7497);
#2281=VERTEX_POINT('',#7502);
#2282=VERTEX_POINT('',#7506);
#2283=VERTEX_POINT('',#7510);
#2284=VERTEX_POINT('',#7534);
#2285=VERTEX_POINT('',#7536);
#2286=VERTEX_POINT('',#7540);
#2287=VERTEX_POINT('',#7543);
#2288=VERTEX_POINT('',#7547);
#2289=VERTEX_POINT('',#7549);
#2290=VERTEX_POINT('',#7554);
#2291=VERTEX_POINT('',#7555);
#2292=VERTEX_POINT('',#7559);
#2293=VERTEX_POINT('',#7561);
#2294=VERTEX_POINT('',#7565);
#2295=VERTEX_POINT('',#7567);
#2296=VERTEX_POINT('',#7574);
#2297=VERTEX_POINT('',#7576);
#2298=VERTEX_POINT('',#7580);
#2299=VERTEX_POINT('',#7583);
#2300=VERTEX_POINT('',#7587);
#2301=VERTEX_POINT('',#7589);
#2302=VERTEX_POINT('',#7597);
#2303=VERTEX_POINT('',#7599);
#2304=VERTEX_POINT('',#7603);
#2305=VERTEX_POINT('',#7606);
#2306=VERTEX_POINT('',#7610);
#2307=VERTEX_POINT('',#7612);
#2308=VERTEX_POINT('',#7617);
#2309=VERTEX_POINT('',#7618);
#2310=VERTEX_POINT('',#7622);
#2311=VERTEX_POINT('',#7624);
#2312=VERTEX_POINT('',#7628);
#2313=VERTEX_POINT('',#7630);
#2314=VERTEX_POINT('',#7637);
#2315=VERTEX_POINT('',#7639);
#2316=VERTEX_POINT('',#7643);
#2317=VERTEX_POINT('',#7646);
#2318=VERTEX_POINT('',#7650);
#2319=VERTEX_POINT('',#7652);
#2320=VERTEX_POINT('',#7660);
#2321=VERTEX_POINT('',#7662);
#2322=VERTEX_POINT('',#7666);
#2323=VERTEX_POINT('',#7669);
#2324=VERTEX_POINT('',#7673);
#2325=VERTEX_POINT('',#7675);
#2326=VERTEX_POINT('',#7680);
#2327=VERTEX_POINT('',#7681);
#2328=VERTEX_POINT('',#7685);
#2329=VERTEX_POINT('',#7687);
#2330=VERTEX_POINT('',#7691);
#2331=VERTEX_POINT('',#7693);
#2332=VERTEX_POINT('',#7700);
#2333=VERTEX_POINT('',#7702);
#2334=VERTEX_POINT('',#7706);
#2335=VERTEX_POINT('',#7709);
#2336=VERTEX_POINT('',#7713);
#2337=VERTEX_POINT('',#7715);
#2338=VERTEX_POINT('',#7723);
#2339=VERTEX_POINT('',#7725);
#2340=VERTEX_POINT('',#7729);
#2341=VERTEX_POINT('',#7732);
#2342=VERTEX_POINT('',#7733);
#2343=VERTEX_POINT('',#7735);
#2344=VERTEX_POINT('',#7737);
#2345=VERTEX_POINT('',#7739);
#2346=VERTEX_POINT('',#7741);
#2347=VERTEX_POINT('',#7744);
#2348=VERTEX_POINT('',#7747);
#2349=VERTEX_POINT('',#7748);
#2350=VERTEX_POINT('',#7750);
#2351=VERTEX_POINT('',#7752);
#2352=VERTEX_POINT('',#7754);
#2353=VERTEX_POINT('',#7756);
#2354=VERTEX_POINT('',#7759);
#2355=VERTEX_POINT('',#7774);
#2356=VERTEX_POINT('',#7777);
#2357=VERTEX_POINT('',#7781);
#2358=VERTEX_POINT('',#7786);
#2359=VERTEX_POINT('',#7790);
#2360=VERTEX_POINT('',#7796);
#2361=VERTEX_POINT('',#7798);
#2362=VERTEX_POINT('',#7801);
#2363=VERTEX_POINT('',#7805);
#2364=VERTEX_POINT('',#7808);
#2365=VERTEX_POINT('',#7812);
#2366=EDGE_CURVE('',#2007,#2007,#1846,.T.);
#2367=EDGE_CURVE('',#2007,#2008,#1138,.T.);
#2368=EDGE_CURVE('',#2008,#2008,#1847,.T.);
#2369=EDGE_CURVE('',#2009,#2010,#1139,.T.);
#2370=EDGE_CURVE('',#2010,#2011,#1140,.T.);
#2371=EDGE_CURVE('',#2012,#2011,#1141,.T.);
#2372=EDGE_CURVE('',#2009,#2012,#1142,.T.);
#2373=EDGE_CURVE('',#2013,#2009,#1143,.T.);
#2374=EDGE_CURVE('',#2014,#2012,#1144,.T.);
#2375=EDGE_CURVE('',#2013,#2014,#1145,.T.);
#2376=EDGE_CURVE('',#2015,#2013,#1146,.T.);
#2377=EDGE_CURVE('',#2016,#2014,#1147,.T.);
#2378=EDGE_CURVE('',#2015,#2016,#1148,.T.);
#2379=EDGE_CURVE('',#2010,#2015,#1149,.T.);
#2380=EDGE_CURVE('',#2011,#2016,#1150,.T.);
#2381=EDGE_CURVE('',#2017,#2018,#1151,.T.);
#2382=EDGE_CURVE('',#2018,#2019,#1152,.T.);
#2383=EDGE_CURVE('',#2020,#2019,#1153,.T.);
#2384=EDGE_CURVE('',#2017,#2020,#1154,.T.);
#2385=EDGE_CURVE('',#2021,#2017,#1155,.T.);
#2386=EDGE_CURVE('',#2022,#2020,#1156,.T.);
#2387=EDGE_CURVE('',#2021,#2022,#1157,.T.);
#2388=EDGE_CURVE('',#2023,#2021,#1158,.T.);
#2389=EDGE_CURVE('',#2024,#2022,#1159,.T.);
#2390=EDGE_CURVE('',#2023,#2024,#1160,.T.);
#2391=EDGE_CURVE('',#2018,#2023,#1161,.T.);
#2392=EDGE_CURVE('',#2019,#2024,#1162,.T.);
#2393=EDGE_CURVE('',#2025,#2026,#1163,.T.);
#2394=EDGE_CURVE('',#2026,#2027,#1164,.T.);
#2395=EDGE_CURVE('',#2028,#2027,#1165,.T.);
#2396=EDGE_CURVE('',#2025,#2028,#1166,.T.);
#2397=EDGE_CURVE('',#2029,#2025,#1167,.T.);
#2398=EDGE_CURVE('',#2030,#2028,#1168,.T.);
#2399=EDGE_CURVE('',#2029,#2030,#1169,.T.);
#2400=EDGE_CURVE('',#2031,#2029,#1170,.T.);
#2401=EDGE_CURVE('',#2032,#2030,#1171,.T.);
#2402=EDGE_CURVE('',#2031,#2032,#1172,.T.);
#2403=EDGE_CURVE('',#2026,#2031,#1173,.T.);
#2404=EDGE_CURVE('',#2027,#2032,#1174,.T.);
#2405=EDGE_CURVE('',#2033,#2033,#1848,.T.);
#2406=EDGE_CURVE('',#2033,#2034,#1175,.T.);
#2407=EDGE_CURVE('',#2034,#2034,#1849,.T.);
#2408=EDGE_CURVE('',#2035,#2035,#1850,.T.);
#2409=EDGE_CURVE('',#2035,#2036,#1176,.T.);
#2410=EDGE_CURVE('',#2036,#2036,#1851,.T.);
#2411=EDGE_CURVE('',#2037,#2037,#1852,.T.);
#2412=EDGE_CURVE('',#2037,#2038,#1177,.T.);
#2413=EDGE_CURVE('',#2038,#2038,#1853,.T.);
#2414=EDGE_CURVE('',#2039,#2040,#1178,.T.);
#2415=EDGE_CURVE('',#2040,#2041,#1179,.T.);
#2416=EDGE_CURVE('',#2042,#2041,#1180,.T.);
#2417=EDGE_CURVE('',#2039,#2042,#1181,.T.);
#2418=EDGE_CURVE('',#2043,#2039,#1182,.T.);
#2419=EDGE_CURVE('',#2044,#2042,#1183,.T.);
#2420=EDGE_CURVE('',#2043,#2044,#1184,.T.);
#2421=EDGE_CURVE('',#2045,#2043,#1185,.T.);
#2422=EDGE_CURVE('',#2046,#2044,#1186,.T.);
#2423=EDGE_CURVE('',#2045,#2046,#1187,.T.);
#2424=EDGE_CURVE('',#2040,#2045,#1188,.T.);
#2425=EDGE_CURVE('',#2041,#2046,#1189,.T.);
#2426=EDGE_CURVE('',#2047,#2048,#1190,.T.);
#2427=EDGE_CURVE('',#2048,#2047,#1854,.T.);
#2428=EDGE_CURVE('',#2049,#2049,#1855,.T.);
#2429=EDGE_CURVE('',#2049,#2050,#1191,.T.);
#2430=EDGE_CURVE('',#2051,#2050,#171,.T.);
#2431=EDGE_CURVE('',#2048,#2051,#172,.T.);
#2432=EDGE_CURVE('',#2052,#2047,#173,.T.);
#2433=EDGE_CURVE('',#2053,#2052,#174,.T.);
#2434=EDGE_CURVE('',#2053,#2054,#1856,.T.);
#2435=EDGE_CURVE('',#2050,#2054,#175,.T.);
#2436=EDGE_CURVE('',#2054,#2053,#1192,.T.);
#2437=EDGE_CURVE('',#2055,#2055,#1857,.T.);
#2438=EDGE_CURVE('',#2055,#2056,#1193,.T.);
#2439=EDGE_CURVE('',#2056,#2056,#1858,.T.);
#2440=EDGE_CURVE('',#2057,#2058,#1194,.T.);
#2441=EDGE_CURVE('',#2058,#2057,#1859,.T.);
#2442=EDGE_CURVE('',#2059,#2059,#1860,.T.);
#2443=EDGE_CURVE('',#2059,#2060,#1195,.T.);
#2444=EDGE_CURVE('',#2061,#2060,#176,.T.);
#2445=EDGE_CURVE('',#2058,#2061,#177,.T.);
#2446=EDGE_CURVE('',#2062,#2057,#178,.T.);
#2447=EDGE_CURVE('',#2063,#2062,#179,.T.);
#2448=EDGE_CURVE('',#2063,#2064,#1861,.T.);
#2449=EDGE_CURVE('',#2060,#2064,#180,.T.);
#2450=EDGE_CURVE('',#2064,#2063,#1196,.T.);
#2451=EDGE_CURVE('',#2065,#2065,#1862,.T.);
#2452=EDGE_CURVE('',#2065,#2066,#1197,.T.);
#2453=EDGE_CURVE('',#2066,#2066,#1863,.T.);
#2454=EDGE_CURVE('',#2067,#2068,#1198,.T.);
#2455=EDGE_CURVE('',#2068,#2067,#1864,.T.);
#2456=EDGE_CURVE('',#2069,#2069,#1865,.T.);
#2457=EDGE_CURVE('',#2069,#2070,#1199,.T.);
#2458=EDGE_CURVE('',#2071,#2070,#181,.T.);
#2459=EDGE_CURVE('',#2068,#2071,#182,.T.);
#2460=EDGE_CURVE('',#2072,#2067,#183,.T.);
#2461=EDGE_CURVE('',#2073,#2072,#184,.T.);
#2462=EDGE_CURVE('',#2073,#2074,#1866,.T.);
#2463=EDGE_CURVE('',#2070,#2074,#185,.T.);
#2464=EDGE_CURVE('',#2074,#2073,#1200,.T.);
#2465=EDGE_CURVE('',#2075,#2075,#1867,.T.);
#2466=EDGE_CURVE('',#2075,#2076,#1201,.T.);
#2467=EDGE_CURVE('',#2076,#2076,#1868,.T.);
#2468=EDGE_CURVE('',#2077,#2077,#1869,.T.);
#2469=EDGE_CURVE('',#2077,#2078,#1202,.T.);
#2470=EDGE_CURVE('',#2078,#2078,#1870,.T.);
#2471=EDGE_CURVE('',#2079,#2079,#186,.T.);
#2472=EDGE_CURVE('',#2080,#2080,#1871,.T.);
#2473=EDGE_CURVE('',#2081,#2081,#1872,.T.);
#2474=EDGE_CURVE('',#2081,#2071,#1203,.T.);
#2475=EDGE_CURVE('',#2072,#2061,#1204,.T.);
#2476=EDGE_CURVE('',#2062,#2051,#1205,.T.);
#2477=EDGE_CURVE('',#2052,#2080,#1206,.T.);
#2478=EDGE_CURVE('',#2082,#2082,#1873,.T.);
#2479=EDGE_CURVE('',#2082,#2083,#1207,.T.);
#2480=EDGE_CURVE('',#2083,#2083,#1874,.T.);
#2481=EDGE_CURVE('',#2084,#2084,#1875,.T.);
#2482=EDGE_CURVE('',#2085,#2085,#1876,.T.);
#2483=EDGE_CURVE('',#2085,#2086,#1208,.T.);
#2484=EDGE_CURVE('',#2086,#2086,#1877,.T.);
#2485=EDGE_CURVE('',#2087,#2087,#1878,.T.);
#2486=EDGE_CURVE('',#2088,#2088,#1879,.T.);
#2487=EDGE_CURVE('',#2088,#2084,#1209,.T.);
#2488=EDGE_CURVE('',#2089,#2089,#1880,.T.);
#2489=EDGE_CURVE('',#2089,#2087,#1210,.T.);
#2490=EDGE_CURVE('',#2090,#2091,#1211,.T.);
#2491=EDGE_CURVE('',#2091,#2092,#1212,.T.);
#2492=EDGE_CURVE('',#2093,#2092,#1213,.T.);
#2493=EDGE_CURVE('',#2090,#2093,#1214,.T.);
#2494=EDGE_CURVE('',#2094,#2090,#1215,.T.);
#2495=EDGE_CURVE('',#2095,#2093,#1216,.T.);
#2496=EDGE_CURVE('',#2094,#2095,#1217,.T.);
#2497=EDGE_CURVE('',#2096,#2094,#1218,.T.);
#2498=EDGE_CURVE('',#2097,#2095,#1219,.T.);
#2499=EDGE_CURVE('',#2096,#2097,#1220,.T.);
#2500=EDGE_CURVE('',#2091,#2096,#1221,.T.);
#2501=EDGE_CURVE('',#2092,#2097,#1222,.T.);
#2502=EDGE_CURVE('',#2098,#2098,#1881,.T.);
#2503=EDGE_CURVE('',#2098,#2099,#1223,.T.);
#2504=EDGE_CURVE('',#2099,#2099,#1882,.T.);
#2505=EDGE_CURVE('',#2100,#2100,#1883,.T.);
#2506=EDGE_CURVE('',#2100,#2101,#1224,.T.);
#2507=EDGE_CURVE('',#2101,#2101,#1884,.T.);
#2508=EDGE_CURVE('',#2102,#2102,#1885,.T.);
#2509=EDGE_CURVE('',#2102,#2103,#1225,.T.);
#2510=EDGE_CURVE('',#2103,#2103,#1886,.T.);
#2511=EDGE_CURVE('',#2104,#2105,#1887,.T.);
#2512=EDGE_CURVE('',#2106,#2106,#1888,.T.);
#2513=EDGE_CURVE('',#2106,#2107,#1226,.T.);
#2514=EDGE_CURVE('',#2107,#2107,#1889,.T.);
#2515=EDGE_CURVE('',#2108,#2108,#1890,.T.);
#2516=EDGE_CURVE('',#2108,#2109,#1227,.T.);
#2517=EDGE_CURVE('',#2109,#2109,#1891,.T.);
#2518=EDGE_CURVE('',#2110,#2110,#1892,.T.);
#2519=EDGE_CURVE('',#2110,#2111,#1228,.T.);
#2520=EDGE_CURVE('',#2111,#2111,#1893,.T.);
#2521=EDGE_CURVE('',#2112,#2112,#1894,.T.);
#2522=EDGE_CURVE('',#2112,#2113,#1229,.T.);
#2523=EDGE_CURVE('',#2113,#2113,#1895,.T.);
#2524=EDGE_CURVE('',#2114,#2115,#1896,.T.);
#2525=EDGE_CURVE('',#2116,#2116,#1897,.T.);
#2526=EDGE_CURVE('',#2116,#2117,#1230,.T.);
#2527=EDGE_CURVE('',#2117,#2117,#1898,.T.);
#2528=EDGE_CURVE('',#2118,#2118,#1899,.T.);
#2529=EDGE_CURVE('',#2118,#2119,#1231,.T.);
#2530=EDGE_CURVE('',#2119,#2119,#1900,.T.);
#2531=EDGE_CURVE('',#2120,#2120,#1901,.T.);
#2532=EDGE_CURVE('',#2120,#2121,#1232,.T.);
#2533=EDGE_CURVE('',#2121,#2121,#1902,.T.);
#2534=EDGE_CURVE('',#2122,#2122,#1903,.T.);
#2535=EDGE_CURVE('',#2122,#2123,#1233,.T.);
#2536=EDGE_CURVE('',#2123,#2123,#1904,.T.);
#2537=EDGE_CURVE('',#2124,#2125,#1905,.T.);
#2538=EDGE_CURVE('',#2126,#2126,#1906,.T.);
#2539=EDGE_CURVE('',#2126,#2127,#1234,.T.);
#2540=EDGE_CURVE('',#2127,#2127,#1907,.T.);
#2541=EDGE_CURVE('',#2128,#2128,#1908,.T.);
#2542=EDGE_CURVE('',#2128,#2129,#1235,.T.);
#2543=EDGE_CURVE('',#2129,#2129,#1909,.T.);
#2544=EDGE_CURVE('',#2130,#2131,#1236,.T.);
#2545=EDGE_CURVE('',#2130,#2132,#1237,.T.);
#2546=EDGE_CURVE('',#2133,#2132,#1238,.T.);
#2547=EDGE_CURVE('',#2131,#2133,#1239,.T.);
#2548=EDGE_CURVE('',#2134,#2130,#1240,.T.);
#2549=EDGE_CURVE('',#2134,#2135,#1241,.T.);
#2550=EDGE_CURVE('',#2132,#2135,#1242,.T.);
#2551=EDGE_CURVE('',#2136,#2134,#1243,.T.);
#2552=EDGE_CURVE('',#2136,#2137,#1244,.T.);
#2553=EDGE_CURVE('',#2135,#2137,#1245,.T.);
#2554=EDGE_CURVE('',#2138,#2136,#1246,.T.);
#2555=EDGE_CURVE('',#2138,#2139,#1247,.T.);
#2556=EDGE_CURVE('',#2137,#2139,#1248,.T.);
#2557=EDGE_CURVE('',#2140,#2138,#1249,.T.);
#2558=EDGE_CURVE('',#2140,#2141,#1250,.T.);
#2559=EDGE_CURVE('',#2139,#2141,#1251,.T.);
#2560=EDGE_CURVE('',#2142,#2140,#1252,.T.);
#2561=EDGE_CURVE('',#2142,#2143,#1253,.T.);
#2562=EDGE_CURVE('',#2141,#2143,#1254,.T.);
#2563=EDGE_CURVE('',#2144,#2142,#1255,.T.);
#2564=EDGE_CURVE('',#2144,#2145,#1256,.T.);
#2565=EDGE_CURVE('',#2143,#2145,#1257,.T.);
#2566=EDGE_CURVE('',#2146,#2144,#1258,.T.);
#2567=EDGE_CURVE('',#2146,#2147,#1259,.T.);
#2568=EDGE_CURVE('',#2145,#2147,#1260,.T.);
#2569=EDGE_CURVE('',#2148,#2146,#1261,.T.);
#2570=EDGE_CURVE('',#2149,#2148,#1262,.T.);
#2571=EDGE_CURVE('',#2147,#2149,#1263,.T.);
#2572=EDGE_CURVE('',#2150,#2151,#1264,.T.);
#2573=EDGE_CURVE('',#2150,#2152,#1265,.T.);
#2574=EDGE_CURVE('',#2153,#2152,#1266,.T.);
#2575=EDGE_CURVE('',#2151,#2153,#1267,.T.);
#2576=EDGE_CURVE('',#2154,#2150,#1268,.T.);
#2577=EDGE_CURVE('',#2154,#2155,#1269,.T.);
#2578=EDGE_CURVE('',#2152,#2155,#1270,.T.);
#2579=EDGE_CURVE('',#2156,#2154,#1271,.T.);
#2580=EDGE_CURVE('',#2156,#2157,#1272,.T.);
#2581=EDGE_CURVE('',#2155,#2157,#1273,.T.);
#2582=EDGE_CURVE('',#2158,#2156,#1274,.T.);
#2583=EDGE_CURVE('',#2158,#2159,#1275,.T.);
#2584=EDGE_CURVE('',#2157,#2159,#1276,.T.);
#2585=EDGE_CURVE('',#2160,#2158,#1277,.T.);
#2586=EDGE_CURVE('',#2160,#2161,#1278,.T.);
#2587=EDGE_CURVE('',#2159,#2161,#1279,.T.);
#2588=EDGE_CURVE('',#2162,#2160,#1280,.T.);
#2589=EDGE_CURVE('',#2162,#2163,#1281,.T.);
#2590=EDGE_CURVE('',#2161,#2163,#1282,.T.);
#2591=EDGE_CURVE('',#2164,#2162,#1283,.T.);
#2592=EDGE_CURVE('',#2164,#2165,#1284,.T.);
#2593=EDGE_CURVE('',#2163,#2165,#1285,.T.);
#2594=EDGE_CURVE('',#2166,#2164,#1286,.T.);
#2595=EDGE_CURVE('',#2166,#2167,#1287,.T.);
#2596=EDGE_CURVE('',#2165,#2167,#1288,.T.);
#2597=EDGE_CURVE('',#2168,#2166,#1289,.T.);
#2598=EDGE_CURVE('',#2169,#2168,#1290,.T.);
#2599=EDGE_CURVE('',#2167,#2169,#1291,.T.);
#2600=EDGE_CURVE('',#2170,#2171,#1292,.T.);
#2601=EDGE_CURVE('',#2170,#2172,#1293,.T.);
#2602=EDGE_CURVE('',#2173,#2172,#1294,.T.);
#2603=EDGE_CURVE('',#2171,#2173,#1295,.T.);
#2604=EDGE_CURVE('',#2174,#2170,#1296,.T.);
#2605=EDGE_CURVE('',#2174,#2175,#1297,.T.);
#2606=EDGE_CURVE('',#2172,#2175,#1298,.T.);
#2607=EDGE_CURVE('',#2176,#2174,#1299,.T.);
#2608=EDGE_CURVE('',#2176,#2177,#1300,.T.);
#2609=EDGE_CURVE('',#2175,#2177,#1301,.T.);
#2610=EDGE_CURVE('',#2178,#2176,#1302,.T.);
#2611=EDGE_CURVE('',#2178,#2179,#1303,.T.);
#2612=EDGE_CURVE('',#2177,#2179,#1304,.T.);
#2613=EDGE_CURVE('',#2180,#2178,#1305,.T.);
#2614=EDGE_CURVE('',#2180,#2181,#1306,.T.);
#2615=EDGE_CURVE('',#2179,#2181,#1307,.T.);
#2616=EDGE_CURVE('',#2182,#2180,#1308,.T.);
#2617=EDGE_CURVE('',#2182,#2183,#1309,.T.);
#2618=EDGE_CURVE('',#2181,#2183,#1310,.T.);
#2619=EDGE_CURVE('',#2184,#2182,#1311,.T.);
#2620=EDGE_CURVE('',#2184,#2185,#1312,.T.);
#2621=EDGE_CURVE('',#2183,#2185,#1313,.T.);
#2622=EDGE_CURVE('',#2186,#2184,#1314,.T.);
#2623=EDGE_CURVE('',#2186,#2187,#1315,.T.);
#2624=EDGE_CURVE('',#2185,#2187,#1316,.T.);
#2625=EDGE_CURVE('',#2188,#2186,#1317,.T.);
#2626=EDGE_CURVE('',#2189,#2188,#1318,.T.);
#2627=EDGE_CURVE('',#2187,#2189,#1319,.T.);
#2628=EDGE_CURVE('',#2190,#2191,#1320,.T.);
#2629=EDGE_CURVE('',#2190,#2192,#1321,.T.);
#2630=EDGE_CURVE('',#2193,#2192,#1322,.T.);
#2631=EDGE_CURVE('',#2191,#2193,#1323,.T.);
#2632=EDGE_CURVE('',#2194,#2190,#1324,.T.);
#2633=EDGE_CURVE('',#2194,#2195,#1325,.T.);
#2634=EDGE_CURVE('',#2192,#2195,#1326,.T.);
#2635=EDGE_CURVE('',#2196,#2194,#1327,.T.);
#2636=EDGE_CURVE('',#2196,#2197,#1328,.T.);
#2637=EDGE_CURVE('',#2195,#2197,#1329,.T.);
#2638=EDGE_CURVE('',#2198,#2196,#1330,.T.);
#2639=EDGE_CURVE('',#2198,#2199,#1331,.T.);
#2640=EDGE_CURVE('',#2197,#2199,#1332,.T.);
#2641=EDGE_CURVE('',#2200,#2198,#1333,.T.);
#2642=EDGE_CURVE('',#2200,#2201,#1334,.T.);
#2643=EDGE_CURVE('',#2199,#2201,#1335,.T.);
#2644=EDGE_CURVE('',#2202,#2200,#1336,.T.);
#2645=EDGE_CURVE('',#2202,#2203,#1337,.T.);
#2646=EDGE_CURVE('',#2201,#2203,#1338,.T.);
#2647=EDGE_CURVE('',#2204,#2202,#1339,.T.);
#2648=EDGE_CURVE('',#2204,#2205,#1340,.T.);
#2649=EDGE_CURVE('',#2203,#2205,#1341,.T.);
#2650=EDGE_CURVE('',#2206,#2204,#1342,.T.);
#2651=EDGE_CURVE('',#2206,#2207,#1343,.T.);
#2652=EDGE_CURVE('',#2205,#2207,#1344,.T.);
#2653=EDGE_CURVE('',#2208,#2206,#1345,.T.);
#2654=EDGE_CURVE('',#2209,#2208,#1346,.T.);
#2655=EDGE_CURVE('',#2207,#2209,#1347,.T.);
#2656=EDGE_CURVE('',#2210,#2210,#1910,.T.);
#2657=EDGE_CURVE('',#2210,#2211,#1348,.T.);
#2658=EDGE_CURVE('',#2211,#2211,#1911,.T.);
#2659=EDGE_CURVE('',#2148,#2212,#1349,.T.);
#2660=EDGE_CURVE('',#2212,#2213,#1350,.T.);
#2661=EDGE_CURVE('',#2149,#2213,#1351,.T.);
#2662=EDGE_CURVE('',#2214,#2133,#1352,.T.);
#2663=EDGE_CURVE('',#2215,#2214,#1353,.T.);
#2664=EDGE_CURVE('',#2215,#2131,#1354,.T.);
#2665=EDGE_CURVE('',#2168,#2215,#1355,.T.);
#2666=EDGE_CURVE('',#2169,#2214,#1356,.T.);
#2667=EDGE_CURVE('',#2216,#2153,#1357,.T.);
#2668=EDGE_CURVE('',#2217,#2216,#1358,.T.);
#2669=EDGE_CURVE('',#2217,#2151,#1359,.T.);
#2670=EDGE_CURVE('',#2188,#2217,#1360,.T.);
#2671=EDGE_CURVE('',#2189,#2216,#1361,.T.);
#2672=EDGE_CURVE('',#2218,#2173,#1362,.T.);
#2673=EDGE_CURVE('',#2219,#2218,#1363,.T.);
#2674=EDGE_CURVE('',#2219,#2171,#1364,.T.);
#2675=EDGE_CURVE('',#2208,#2219,#1365,.T.);
#2676=EDGE_CURVE('',#2209,#2218,#1366,.T.);
#2677=EDGE_CURVE('',#2213,#2193,#1367,.T.);
#2678=EDGE_CURVE('',#2212,#2191,#1368,.T.);
#2679=EDGE_CURVE('',#2220,#2220,#1912,.T.);
#2680=EDGE_CURVE('',#2220,#2221,#1369,.T.);
#2681=EDGE_CURVE('',#2221,#2221,#1913,.T.);
#2682=EDGE_CURVE('',#2221,#2222,#1370,.T.);
#2683=EDGE_CURVE('',#2222,#2222,#1914,.T.);
#2684=EDGE_CURVE('',#2223,#2223,#1915,.T.);
#2685=EDGE_CURVE('',#2223,#2224,#1371,.T.);
#2686=EDGE_CURVE('',#2224,#2224,#1916,.T.);
#2687=EDGE_CURVE('',#2225,#2226,#1372,.T.);
#2688=EDGE_CURVE('',#2226,#2227,#1373,.T.);
#2689=EDGE_CURVE('',#2227,#2228,#1374,.T.);
#2690=EDGE_CURVE('',#2225,#2228,#1375,.T.);
#2691=EDGE_CURVE('',#2226,#2229,#1376,.T.);
#2692=EDGE_CURVE('',#2229,#2230,#1377,.T.);
#2693=EDGE_CURVE('',#2230,#2227,#1378,.T.);
#2694=EDGE_CURVE('',#2229,#2231,#1379,.T.);
#2695=EDGE_CURVE('',#2231,#2232,#1380,.T.);
#2696=EDGE_CURVE('',#2232,#2230,#1381,.T.);
#2697=EDGE_CURVE('',#2231,#2233,#1382,.T.);
#2698=EDGE_CURVE('',#2233,#2234,#1383,.T.);
#2699=EDGE_CURVE('',#2234,#2232,#1384,.T.);
#2700=EDGE_CURVE('',#2233,#2235,#1385,.T.);
#2701=EDGE_CURVE('',#2235,#2236,#1386,.T.);
#2702=EDGE_CURVE('',#2236,#2234,#1387,.T.);
#2703=EDGE_CURVE('',#2235,#2225,#1388,.T.);
#2704=EDGE_CURVE('',#2228,#2236,#1389,.T.);
#2705=EDGE_CURVE('',#2237,#2237,#1917,.T.);
#2706=EDGE_CURVE('',#2238,#2238,#1918,.T.);
#2707=EDGE_CURVE('',#2239,#2239,#1919,.T.);
#2708=EDGE_CURVE('',#2239,#2238,#1390,.T.);
#2709=EDGE_CURVE('',#2240,#2240,#1920,.T.);
#2710=EDGE_CURVE('',#2240,#2239,#1391,.T.);
#2711=EDGE_CURVE('',#2241,#2241,#1921,.T.);
#2712=EDGE_CURVE('',#2241,#2240,#1392,.T.);
#2713=EDGE_CURVE('',#2242,#2242,#1922,.T.);
#2714=EDGE_CURVE('',#2243,#2243,#1923,.F.);
#2715=EDGE_CURVE('',#2243,#2242,#1393,.T.);
#2716=EDGE_CURVE('',#2237,#2243,#1394,.T.);
#2717=EDGE_CURVE('',#2244,#2244,#1924,.T.);
#2718=EDGE_CURVE('',#2245,#2245,#1925,.T.);
#2719=EDGE_CURVE('',#2245,#2244,#1395,.T.);
#2720=EDGE_CURVE('',#2246,#2246,#1926,.T.);
#2721=EDGE_CURVE('',#2246,#2245,#1396,.T.);
#2722=EDGE_CURVE('',#2247,#2247,#1927,.T.);
#2723=EDGE_CURVE('',#2247,#2246,#1397,.T.);
#2724=EDGE_CURVE('',#2248,#2248,#1928,.T.);
#2725=EDGE_CURVE('',#2249,#2249,#1929,.F.);
#2726=EDGE_CURVE('',#2249,#2248,#1398,.T.);
#2727=EDGE_CURVE('',#2250,#2250,#1930,.F.);
#2728=EDGE_CURVE('',#2250,#2249,#1399,.T.);
#2729=EDGE_CURVE('',#2251,#2251,#1931,.T.);
#2730=EDGE_CURVE('',#2251,#2250,#1400,.T.);
#2731=EDGE_CURVE('',#2252,#2253,#1401,.T.);
#2732=EDGE_CURVE('',#2253,#2254,#1402,.T.);
#2733=EDGE_CURVE('',#2254,#2255,#1403,.T.);
#2734=EDGE_CURVE('',#2252,#2255,#1404,.T.);
#2735=EDGE_CURVE('',#2253,#2256,#1405,.T.);
#2736=EDGE_CURVE('',#2256,#2257,#1406,.T.);
#2737=EDGE_CURVE('',#2257,#2254,#1407,.T.);
#2738=EDGE_CURVE('',#2256,#2258,#1408,.T.);
#2739=EDGE_CURVE('',#2258,#2259,#1409,.T.);
#2740=EDGE_CURVE('',#2259,#2257,#1410,.T.);
#2741=EDGE_CURVE('',#2258,#2260,#1411,.T.);
#2742=EDGE_CURVE('',#2260,#2261,#1412,.T.);
#2743=EDGE_CURVE('',#2261,#2259,#1413,.T.);
#2744=EDGE_CURVE('',#2260,#2262,#1414,.T.);
#2745=EDGE_CURVE('',#2262,#2263,#1415,.T.);
#2746=EDGE_CURVE('',#2263,#2261,#1416,.T.);
#2747=EDGE_CURVE('',#2262,#2252,#1417,.T.);
#2748=EDGE_CURVE('',#2255,#2263,#1418,.T.);
#2749=EDGE_CURVE('',#2264,#2265,#1419,.T.);
#2750=EDGE_CURVE('',#2265,#2266,#1420,.T.);
#2751=EDGE_CURVE('',#2266,#2267,#1421,.T.);
#2752=EDGE_CURVE('',#2267,#2268,#1422,.T.);
#2753=EDGE_CURVE('',#2268,#2269,#1423,.T.);
#2754=EDGE_CURVE('',#2269,#2264,#1424,.T.);
#2755=EDGE_CURVE('',#2270,#2270,#1932,.T.);
#2756=EDGE_CURVE('',#2271,#2272,#1425,.T.);
#2757=EDGE_CURVE('',#2272,#2273,#1426,.T.);
#2758=EDGE_CURVE('',#2273,#2274,#1427,.T.);
#2759=EDGE_CURVE('',#2274,#2275,#1428,.T.);
#2760=EDGE_CURVE('',#2275,#2276,#1429,.T.);
#2761=EDGE_CURVE('',#2276,#2271,#1430,.T.);
#2762=EDGE_CURVE('',#2277,#2277,#1933,.T.);
#2763=EDGE_CURVE('',#2271,#2265,#1431,.T.);
#2764=EDGE_CURVE('',#2266,#2276,#1432,.T.);
#2765=EDGE_CURVE('',#2267,#2275,#1433,.T.);
#2766=EDGE_CURVE('',#2268,#2274,#1434,.T.);
#2767=EDGE_CURVE('',#2269,#2273,#1435,.T.);
#2768=EDGE_CURVE('',#2264,#2272,#1436,.T.);
#2769=EDGE_CURVE('',#2277,#2278,#1437,.T.);
#2770=EDGE_CURVE('',#2278,#2278,#1934,.T.);
#2771=EDGE_CURVE('',#2279,#2279,#1935,.T.);
#2772=EDGE_CURVE('',#2280,#2280,#1936,.T.);
#2773=EDGE_CURVE('',#2278,#2279,#1438,.T.);
#2774=EDGE_CURVE('',#2281,#2281,#1937,.T.);
#2775=EDGE_CURVE('',#2281,#2270,#1439,.T.);
#2776=EDGE_CURVE('',#2282,#2282,#1938,.T.);
#2777=EDGE_CURVE('',#2282,#2281,#1440,.T.);
#2778=EDGE_CURVE('',#2283,#2283,#1939,.T.);
#2779=EDGE_CURVE('',#2283,#2280,#1441,.T.);
#2780=EDGE_CURVE('',#2284,#2284,#1940,.T.);
#2781=EDGE_CURVE('',#2284,#2285,#1442,.T.);
#2782=EDGE_CURVE('',#2285,#2285,#1941,.T.);
#2783=EDGE_CURVE('',#2286,#2286,#1942,.T.);
#2784=EDGE_CURVE('',#2286,#2287,#1443,.T.);
#2785=EDGE_CURVE('',#2287,#2287,#1943,.T.);
#2786=EDGE_CURVE('',#2288,#2288,#1944,.T.);
#2787=EDGE_CURVE('',#2288,#2289,#1444,.T.);
#2788=EDGE_CURVE('',#2289,#2289,#1945,.T.);
#2789=EDGE_CURVE('',#2290,#2291,#1946,.T.);
#2790=EDGE_CURVE('',#2292,#2292,#1947,.T.);
#2791=EDGE_CURVE('',#2292,#2293,#1445,.T.);
#2792=EDGE_CURVE('',#2293,#2293,#1948,.T.);
#2793=EDGE_CURVE('',#2294,#2294,#1949,.T.);
#2794=EDGE_CURVE('',#2294,#2295,#1446,.T.);
#2795=EDGE_CURVE('',#2295,#2295,#1950,.T.);
#2796=EDGE_CURVE('',#2296,#2296,#1951,.T.);
#2797=EDGE_CURVE('',#2296,#2297,#1447,.T.);
#2798=EDGE_CURVE('',#2297,#2297,#1952,.T.);
#2799=EDGE_CURVE('',#2298,#2298,#1953,.T.);
#2800=EDGE_CURVE('',#2298,#2299,#1448,.T.);
#2801=EDGE_CURVE('',#2299,#2299,#1954,.T.);
#2802=EDGE_CURVE('',#2300,#2300,#1955,.T.);
#2803=EDGE_CURVE('',#2300,#2301,#1449,.T.);
#2804=EDGE_CURVE('',#2301,#2301,#1956,.T.);
#2805=EDGE_CURVE('',#2302,#2302,#1957,.T.);
#2806=EDGE_CURVE('',#2302,#2303,#1450,.T.);
#2807=EDGE_CURVE('',#2303,#2303,#1958,.T.);
#2808=EDGE_CURVE('',#2304,#2304,#1959,.T.);
#2809=EDGE_CURVE('',#2304,#2305,#1451,.T.);
#2810=EDGE_CURVE('',#2305,#2305,#1960,.T.);
#2811=EDGE_CURVE('',#2306,#2306,#1961,.T.);
#2812=EDGE_CURVE('',#2306,#2307,#1452,.T.);
#2813=EDGE_CURVE('',#2307,#2307,#1962,.T.);
#2814=EDGE_CURVE('',#2308,#2309,#1963,.T.);
#2815=EDGE_CURVE('',#2310,#2310,#1964,.T.);
#2816=EDGE_CURVE('',#2310,#2311,#1453,.T.);
#2817=EDGE_CURVE('',#2311,#2311,#1965,.T.);
#2818=EDGE_CURVE('',#2312,#2312,#1966,.T.);
#2819=EDGE_CURVE('',#2312,#2313,#1454,.T.);
#2820=EDGE_CURVE('',#2313,#2313,#1967,.T.);
#2821=EDGE_CURVE('',#2314,#2314,#1968,.T.);
#2822=EDGE_CURVE('',#2314,#2315,#1455,.T.);
#2823=EDGE_CURVE('',#2315,#2315,#1969,.T.);
#2824=EDGE_CURVE('',#2316,#2316,#1970,.T.);
#2825=EDGE_CURVE('',#2316,#2317,#1456,.T.);
#2826=EDGE_CURVE('',#2317,#2317,#1971,.T.);
#2827=EDGE_CURVE('',#2318,#2318,#1972,.T.);
#2828=EDGE_CURVE('',#2318,#2319,#1457,.T.);
#2829=EDGE_CURVE('',#2319,#2319,#1973,.T.);
#2830=EDGE_CURVE('',#2320,#2320,#1974,.T.);
#2831=EDGE_CURVE('',#2320,#2321,#1458,.T.);
#2832=EDGE_CURVE('',#2321,#2321,#1975,.T.);
#2833=EDGE_CURVE('',#2322,#2322,#1976,.T.);
#2834=EDGE_CURVE('',#2322,#2323,#1459,.T.);
#2835=EDGE_CURVE('',#2323,#2323,#1977,.T.);
#2836=EDGE_CURVE('',#2324,#2324,#1978,.T.);
#2837=EDGE_CURVE('',#2324,#2325,#1460,.T.);
#2838=EDGE_CURVE('',#2325,#2325,#1979,.T.);
#2839=EDGE_CURVE('',#2326,#2327,#1980,.T.);
#2840=EDGE_CURVE('',#2328,#2328,#1981,.T.);
#2841=EDGE_CURVE('',#2328,#2329,#1461,.T.);
#2842=EDGE_CURVE('',#2329,#2329,#1982,.T.);
#2843=EDGE_CURVE('',#2330,#2330,#1983,.T.);
#2844=EDGE_CURVE('',#2330,#2331,#1462,.T.);
#2845=EDGE_CURVE('',#2331,#2331,#1984,.T.);
#2846=EDGE_CURVE('',#2332,#2332,#1985,.T.);
#2847=EDGE_CURVE('',#2332,#2333,#1463,.T.);
#2848=EDGE_CURVE('',#2333,#2333,#1986,.T.);
#2849=EDGE_CURVE('',#2334,#2334,#1987,.T.);
#2850=EDGE_CURVE('',#2334,#2335,#1464,.T.);
#2851=EDGE_CURVE('',#2335,#2335,#1988,.T.);
#2852=EDGE_CURVE('',#2336,#2336,#1989,.T.);
#2853=EDGE_CURVE('',#2336,#2337,#1465,.T.);
#2854=EDGE_CURVE('',#2337,#2337,#1990,.T.);
#2855=EDGE_CURVE('',#2338,#2338,#1991,.T.);
#2856=EDGE_CURVE('',#2338,#2339,#1466,.T.);
#2857=EDGE_CURVE('',#2339,#2339,#1992,.T.);
#2858=EDGE_CURVE('',#2340,#2340,#1993,.T.);
#2859=EDGE_CURVE('',#2341,#2342,#1467,.T.);
#2860=EDGE_CURVE('',#2342,#2343,#1468,.T.);
#2861=EDGE_CURVE('',#2343,#2344,#1469,.T.);
#2862=EDGE_CURVE('',#2344,#2345,#1470,.T.);
#2863=EDGE_CURVE('',#2345,#2346,#1471,.T.);
#2864=EDGE_CURVE('',#2346,#2341,#1472,.T.);
#2865=EDGE_CURVE('',#2347,#2347,#1994,.T.);
#2866=EDGE_CURVE('',#2348,#2349,#1473,.T.);
#2867=EDGE_CURVE('',#2350,#2348,#1474,.T.);
#2868=EDGE_CURVE('',#2351,#2350,#1475,.T.);
#2869=EDGE_CURVE('',#2352,#2351,#1476,.T.);
#2870=EDGE_CURVE('',#2353,#2352,#1477,.T.);
#2871=EDGE_CURVE('',#2349,#2353,#1478,.T.);
#2872=EDGE_CURVE('',#2354,#2354,#1995,.T.);
#2873=EDGE_CURVE('',#2348,#2341,#1479,.T.);
#2874=EDGE_CURVE('',#2350,#2346,#1480,.T.);
#2875=EDGE_CURVE('',#2351,#2345,#1481,.T.);
#2876=EDGE_CURVE('',#2352,#2344,#1482,.T.);
#2877=EDGE_CURVE('',#2353,#2343,#1483,.T.);
#2878=EDGE_CURVE('',#2349,#2342,#1484,.T.);
#2879=EDGE_CURVE('',#2355,#2355,#1996,.T.);
#2880=EDGE_CURVE('',#2355,#2356,#1485,.T.);
#2881=EDGE_CURVE('',#2356,#2356,#1997,.T.);
#2882=EDGE_CURVE('',#2357,#2357,#1998,.T.);
#2883=EDGE_CURVE('',#2347,#2357,#1486,.T.);
#2884=EDGE_CURVE('',#2358,#2358,#1999,.T.);
#2885=EDGE_CURVE('',#2358,#2354,#1487,.T.);
#2886=EDGE_CURVE('',#2359,#2359,#2000,.T.);
#2887=EDGE_CURVE('',#2359,#2340,#1488,.T.);
#2888=EDGE_CURVE('',#2360,#2360,#2001,.T.);
#2889=EDGE_CURVE('',#2361,#2361,#2002,.T.);
#2890=EDGE_CURVE('',#2362,#2362,#2003,.T.);
#2891=EDGE_CURVE('',#2362,#2360,#1489,.T.);
#2892=EDGE_CURVE('',#2363,#2363,#2004,.T.);
#2893=EDGE_CURVE('',#2364,#2364,#2005,.T.);
#2894=EDGE_CURVE('',#2364,#2363,#1490,.T.);
#2895=EDGE_CURVE('',#2365,#2365,#2006,.T.);
#2896=EDGE_CURVE('',#2365,#2361,#1491,.T.);
#2897=ORIENTED_EDGE('',*,*,#2366,.F.);
#2898=ORIENTED_EDGE('',*,*,#2367,.T.);
#2899=ORIENTED_EDGE('',*,*,#2368,.F.);
#2900=ORIENTED_EDGE('',*,*,#2367,.F.);
#2901=ORIENTED_EDGE('',*,*,#2369,.T.);
#2902=ORIENTED_EDGE('',*,*,#2370,.T.);
#2903=ORIENTED_EDGE('',*,*,#2371,.F.);
#2904=ORIENTED_EDGE('',*,*,#2372,.F.);
#2905=ORIENTED_EDGE('',*,*,#2373,.T.);
#2906=ORIENTED_EDGE('',*,*,#2372,.T.);
#2907=ORIENTED_EDGE('',*,*,#2374,.F.);
#2908=ORIENTED_EDGE('',*,*,#2375,.F.);
#2909=ORIENTED_EDGE('',*,*,#2376,.T.);
#2910=ORIENTED_EDGE('',*,*,#2375,.T.);
#2911=ORIENTED_EDGE('',*,*,#2377,.F.);
#2912=ORIENTED_EDGE('',*,*,#2378,.F.);
#2913=ORIENTED_EDGE('',*,*,#2379,.T.);
#2914=ORIENTED_EDGE('',*,*,#2378,.T.);
#2915=ORIENTED_EDGE('',*,*,#2380,.F.);
#2916=ORIENTED_EDGE('',*,*,#2370,.F.);
#2917=ORIENTED_EDGE('',*,*,#2380,.T.);
#2918=ORIENTED_EDGE('',*,*,#2377,.T.);
#2919=ORIENTED_EDGE('',*,*,#2374,.T.);
#2920=ORIENTED_EDGE('',*,*,#2371,.T.);
#2921=ORIENTED_EDGE('',*,*,#2368,.T.);
#2922=ORIENTED_EDGE('',*,*,#2379,.F.);
#2923=ORIENTED_EDGE('',*,*,#2369,.F.);
#2924=ORIENTED_EDGE('',*,*,#2373,.F.);
#2925=ORIENTED_EDGE('',*,*,#2376,.F.);
#2926=ORIENTED_EDGE('',*,*,#2366,.T.);
#2927=ORIENTED_EDGE('',*,*,#2381,.T.);
#2928=ORIENTED_EDGE('',*,*,#2382,.T.);
#2929=ORIENTED_EDGE('',*,*,#2383,.F.);
#2930=ORIENTED_EDGE('',*,*,#2384,.F.);
#2931=ORIENTED_EDGE('',*,*,#2385,.T.);
#2932=ORIENTED_EDGE('',*,*,#2384,.T.);
#2933=ORIENTED_EDGE('',*,*,#2386,.F.);
#2934=ORIENTED_EDGE('',*,*,#2387,.F.);
#2935=ORIENTED_EDGE('',*,*,#2388,.T.);
#2936=ORIENTED_EDGE('',*,*,#2387,.T.);
#2937=ORIENTED_EDGE('',*,*,#2389,.F.);
#2938=ORIENTED_EDGE('',*,*,#2390,.F.);
#2939=ORIENTED_EDGE('',*,*,#2391,.T.);
#2940=ORIENTED_EDGE('',*,*,#2390,.T.);
#2941=ORIENTED_EDGE('',*,*,#2392,.F.);
#2942=ORIENTED_EDGE('',*,*,#2382,.F.);
#2943=ORIENTED_EDGE('',*,*,#2392,.T.);
#2944=ORIENTED_EDGE('',*,*,#2389,.T.);
#2945=ORIENTED_EDGE('',*,*,#2386,.T.);
#2946=ORIENTED_EDGE('',*,*,#2383,.T.);
#2947=ORIENTED_EDGE('',*,*,#2391,.F.);
#2948=ORIENTED_EDGE('',*,*,#2381,.F.);
#2949=ORIENTED_EDGE('',*,*,#2385,.F.);
#2950=ORIENTED_EDGE('',*,*,#2388,.F.);
#2951=ORIENTED_EDGE('',*,*,#2393,.T.);
#2952=ORIENTED_EDGE('',*,*,#2394,.T.);
#2953=ORIENTED_EDGE('',*,*,#2395,.F.);
#2954=ORIENTED_EDGE('',*,*,#2396,.F.);
#2955=ORIENTED_EDGE('',*,*,#2397,.T.);
#2956=ORIENTED_EDGE('',*,*,#2396,.T.);
#2957=ORIENTED_EDGE('',*,*,#2398,.F.);
#2958=ORIENTED_EDGE('',*,*,#2399,.F.);
#2959=ORIENTED_EDGE('',*,*,#2400,.T.);
#2960=ORIENTED_EDGE('',*,*,#2399,.T.);
#2961=ORIENTED_EDGE('',*,*,#2401,.F.);
#2962=ORIENTED_EDGE('',*,*,#2402,.F.);
#2963=ORIENTED_EDGE('',*,*,#2403,.T.);
#2964=ORIENTED_EDGE('',*,*,#2402,.T.);
#2965=ORIENTED_EDGE('',*,*,#2404,.F.);
#2966=ORIENTED_EDGE('',*,*,#2394,.F.);
#2967=ORIENTED_EDGE('',*,*,#2404,.T.);
#2968=ORIENTED_EDGE('',*,*,#2401,.T.);
#2969=ORIENTED_EDGE('',*,*,#2398,.T.);
#2970=ORIENTED_EDGE('',*,*,#2395,.T.);
#2971=ORIENTED_EDGE('',*,*,#2403,.F.);
#2972=ORIENTED_EDGE('',*,*,#2393,.F.);
#2973=ORIENTED_EDGE('',*,*,#2397,.F.);
#2974=ORIENTED_EDGE('',*,*,#2400,.F.);
#2975=ORIENTED_EDGE('',*,*,#2405,.F.);
#2976=ORIENTED_EDGE('',*,*,#2406,.T.);
#2977=ORIENTED_EDGE('',*,*,#2407,.F.);
#2978=ORIENTED_EDGE('',*,*,#2406,.F.);
#2979=ORIENTED_EDGE('',*,*,#2408,.F.);
#2980=ORIENTED_EDGE('',*,*,#2409,.T.);
#2981=ORIENTED_EDGE('',*,*,#2410,.F.);
#2982=ORIENTED_EDGE('',*,*,#2409,.F.);
#2983=ORIENTED_EDGE('',*,*,#2411,.F.);
#2984=ORIENTED_EDGE('',*,*,#2412,.T.);
#2985=ORIENTED_EDGE('',*,*,#2413,.F.);
#2986=ORIENTED_EDGE('',*,*,#2412,.F.);
#2987=ORIENTED_EDGE('',*,*,#2414,.T.);
#2988=ORIENTED_EDGE('',*,*,#2415,.T.);
#2989=ORIENTED_EDGE('',*,*,#2416,.F.);
#2990=ORIENTED_EDGE('',*,*,#2417,.F.);
#2991=ORIENTED_EDGE('',*,*,#2418,.T.);
#2992=ORIENTED_EDGE('',*,*,#2417,.T.);
#2993=ORIENTED_EDGE('',*,*,#2419,.F.);
#2994=ORIENTED_EDGE('',*,*,#2420,.F.);
#2995=ORIENTED_EDGE('',*,*,#2421,.T.);
#2996=ORIENTED_EDGE('',*,*,#2420,.T.);
#2997=ORIENTED_EDGE('',*,*,#2422,.F.);
#2998=ORIENTED_EDGE('',*,*,#2423,.F.);
#2999=ORIENTED_EDGE('',*,*,#2424,.T.);
#3000=ORIENTED_EDGE('',*,*,#2423,.T.);
#3001=ORIENTED_EDGE('',*,*,#2425,.F.);
#3002=ORIENTED_EDGE('',*,*,#2415,.F.);
#3003=ORIENTED_EDGE('',*,*,#2425,.T.);
#3004=ORIENTED_EDGE('',*,*,#2422,.T.);
#3005=ORIENTED_EDGE('',*,*,#2419,.T.);
#3006=ORIENTED_EDGE('',*,*,#2416,.T.);
#3007=ORIENTED_EDGE('',*,*,#2407,.T.);
#3008=ORIENTED_EDGE('',*,*,#2410,.T.);
#3009=ORIENTED_EDGE('',*,*,#2413,.T.);
#3010=ORIENTED_EDGE('',*,*,#2424,.F.);
#3011=ORIENTED_EDGE('',*,*,#2414,.F.);
#3012=ORIENTED_EDGE('',*,*,#2418,.F.);
#3013=ORIENTED_EDGE('',*,*,#2421,.F.);
#3014=ORIENTED_EDGE('',*,*,#2405,.T.);
#3015=ORIENTED_EDGE('',*,*,#2408,.T.);
#3016=ORIENTED_EDGE('',*,*,#2411,.T.);
#3017=ORIENTED_EDGE('',*,*,#2426,.F.);
#3018=ORIENTED_EDGE('',*,*,#2427,.F.);
#3019=ORIENTED_EDGE('',*,*,#2428,.F.);
#3020=ORIENTED_EDGE('',*,*,#2429,.T.);
#3021=ORIENTED_EDGE('',*,*,#2430,.F.);
#3022=ORIENTED_EDGE('',*,*,#2431,.F.);
#3023=ORIENTED_EDGE('',*,*,#2427,.T.);
#3024=ORIENTED_EDGE('',*,*,#2432,.F.);
#3025=ORIENTED_EDGE('',*,*,#2433,.F.);
#3026=ORIENTED_EDGE('',*,*,#2434,.T.);
#3027=ORIENTED_EDGE('',*,*,#2435,.F.);
#3028=ORIENTED_EDGE('',*,*,#2429,.F.);
#3029=ORIENTED_EDGE('',*,*,#2436,.F.);
#3030=ORIENTED_EDGE('',*,*,#2434,.F.);
#3031=ORIENTED_EDGE('',*,*,#2437,.F.);
#3032=ORIENTED_EDGE('',*,*,#2438,.T.);
#3033=ORIENTED_EDGE('',*,*,#2439,.T.);
#3034=ORIENTED_EDGE('',*,*,#2438,.F.);
#3035=ORIENTED_EDGE('',*,*,#2439,.F.);
#3036=ORIENTED_EDGE('',*,*,#2428,.T.);
#3037=ORIENTED_EDGE('',*,*,#2440,.F.);
#3038=ORIENTED_EDGE('',*,*,#2441,.F.);
#3039=ORIENTED_EDGE('',*,*,#2442,.F.);
#3040=ORIENTED_EDGE('',*,*,#2443,.T.);
#3041=ORIENTED_EDGE('',*,*,#2444,.F.);
#3042=ORIENTED_EDGE('',*,*,#2445,.F.);
#3043=ORIENTED_EDGE('',*,*,#2441,.T.);
#3044=ORIENTED_EDGE('',*,*,#2446,.F.);
#3045=ORIENTED_EDGE('',*,*,#2447,.F.);
#3046=ORIENTED_EDGE('',*,*,#2448,.T.);
#3047=ORIENTED_EDGE('',*,*,#2449,.F.);
#3048=ORIENTED_EDGE('',*,*,#2443,.F.);
#3049=ORIENTED_EDGE('',*,*,#2450,.F.);
#3050=ORIENTED_EDGE('',*,*,#2448,.F.);
#3051=ORIENTED_EDGE('',*,*,#2451,.F.);
#3052=ORIENTED_EDGE('',*,*,#2452,.T.);
#3053=ORIENTED_EDGE('',*,*,#2453,.T.);
#3054=ORIENTED_EDGE('',*,*,#2452,.F.);
#3055=ORIENTED_EDGE('',*,*,#2453,.F.);
#3056=ORIENTED_EDGE('',*,*,#2442,.T.);
#3057=ORIENTED_EDGE('',*,*,#2454,.F.);
#3058=ORIENTED_EDGE('',*,*,#2455,.F.);
#3059=ORIENTED_EDGE('',*,*,#2456,.F.);
#3060=ORIENTED_EDGE('',*,*,#2457,.T.);
#3061=ORIENTED_EDGE('',*,*,#2458,.F.);
#3062=ORIENTED_EDGE('',*,*,#2459,.F.);
#3063=ORIENTED_EDGE('',*,*,#2455,.T.);
#3064=ORIENTED_EDGE('',*,*,#2460,.F.);
#3065=ORIENTED_EDGE('',*,*,#2461,.F.);
#3066=ORIENTED_EDGE('',*,*,#2462,.T.);
#3067=ORIENTED_EDGE('',*,*,#2463,.F.);
#3068=ORIENTED_EDGE('',*,*,#2457,.F.);
#3069=ORIENTED_EDGE('',*,*,#2464,.F.);
#3070=ORIENTED_EDGE('',*,*,#2462,.F.);
#3071=ORIENTED_EDGE('',*,*,#2465,.F.);
#3072=ORIENTED_EDGE('',*,*,#2466,.T.);
#3073=ORIENTED_EDGE('',*,*,#2467,.T.);
#3074=ORIENTED_EDGE('',*,*,#2466,.F.);
#3075=ORIENTED_EDGE('',*,*,#2467,.F.);
#3076=ORIENTED_EDGE('',*,*,#2456,.T.);
#3077=ORIENTED_EDGE('',*,*,#2468,.F.);
#3078=ORIENTED_EDGE('',*,*,#2469,.T.);
#3079=ORIENTED_EDGE('',*,*,#2470,.F.);
#3080=ORIENTED_EDGE('',*,*,#2469,.F.);
#3081=ORIENTED_EDGE('',*,*,#2471,.F.);
#3082=ORIENTED_EDGE('',*,*,#2468,.T.);
#3083=ORIENTED_EDGE('',*,*,#2472,.F.);
#3084=ORIENTED_EDGE('',*,*,#2473,.F.);
#3085=ORIENTED_EDGE('',*,*,#2474,.T.);
#3086=ORIENTED_EDGE('',*,*,#2458,.T.);
#3087=ORIENTED_EDGE('',*,*,#2463,.T.);
#3088=ORIENTED_EDGE('',*,*,#2464,.T.);
#3089=ORIENTED_EDGE('',*,*,#2461,.T.);
#3090=ORIENTED_EDGE('',*,*,#2475,.T.);
#3091=ORIENTED_EDGE('',*,*,#2444,.T.);
#3092=ORIENTED_EDGE('',*,*,#2449,.T.);
#3093=ORIENTED_EDGE('',*,*,#2450,.T.);
#3094=ORIENTED_EDGE('',*,*,#2447,.T.);
#3095=ORIENTED_EDGE('',*,*,#2476,.T.);
#3096=ORIENTED_EDGE('',*,*,#2430,.T.);
#3097=ORIENTED_EDGE('',*,*,#2435,.T.);
#3098=ORIENTED_EDGE('',*,*,#2436,.T.);
#3099=ORIENTED_EDGE('',*,*,#2433,.T.);
#3100=ORIENTED_EDGE('',*,*,#2477,.T.);
#3101=ORIENTED_EDGE('',*,*,#2472,.T.);
#3102=ORIENTED_EDGE('',*,*,#2477,.F.);
#3103=ORIENTED_EDGE('',*,*,#2432,.T.);
#3104=ORIENTED_EDGE('',*,*,#2426,.T.);
#3105=ORIENTED_EDGE('',*,*,#2431,.T.);
#3106=ORIENTED_EDGE('',*,*,#2476,.F.);
#3107=ORIENTED_EDGE('',*,*,#2446,.T.);
#3108=ORIENTED_EDGE('',*,*,#2440,.T.);
#3109=ORIENTED_EDGE('',*,*,#2445,.T.);
#3110=ORIENTED_EDGE('',*,*,#2475,.F.);
#3111=ORIENTED_EDGE('',*,*,#2460,.T.);
#3112=ORIENTED_EDGE('',*,*,#2454,.T.);
#3113=ORIENTED_EDGE('',*,*,#2459,.T.);
#3114=ORIENTED_EDGE('',*,*,#2474,.F.);
#3115=ORIENTED_EDGE('',*,*,#2478,.F.);
#3116=ORIENTED_EDGE('',*,*,#2479,.T.);
#3117=ORIENTED_EDGE('',*,*,#2480,.F.);
#3118=ORIENTED_EDGE('',*,*,#2479,.F.);
#3119=ORIENTED_EDGE('',*,*,#2478,.T.);
#3120=ORIENTED_EDGE('',*,*,#2481,.F.);
#3121=ORIENTED_EDGE('',*,*,#2482,.F.);
#3122=ORIENTED_EDGE('',*,*,#2483,.T.);
#3123=ORIENTED_EDGE('',*,*,#2484,.F.);
#3124=ORIENTED_EDGE('',*,*,#2483,.F.);
#3125=ORIENTED_EDGE('',*,*,#2471,.T.);
#3126=ORIENTED_EDGE('',*,*,#2482,.T.);
#3127=ORIENTED_EDGE('',*,*,#2485,.F.);
#3128=ORIENTED_EDGE('',*,*,#2486,.F.);
#3129=ORIENTED_EDGE('',*,*,#2487,.T.);
#3130=ORIENTED_EDGE('',*,*,#2481,.T.);
#3131=ORIENTED_EDGE('',*,*,#2487,.F.);
#3132=ORIENTED_EDGE('',*,*,#2488,.F.);
#3133=ORIENTED_EDGE('',*,*,#2489,.T.);
#3134=ORIENTED_EDGE('',*,*,#2485,.T.);
#3135=ORIENTED_EDGE('',*,*,#2489,.F.);
#3136=ORIENTED_EDGE('',*,*,#2490,.T.);
#3137=ORIENTED_EDGE('',*,*,#2491,.T.);
#3138=ORIENTED_EDGE('',*,*,#2492,.F.);
#3139=ORIENTED_EDGE('',*,*,#2493,.F.);
#3140=ORIENTED_EDGE('',*,*,#2494,.T.);
#3141=ORIENTED_EDGE('',*,*,#2493,.T.);
#3142=ORIENTED_EDGE('',*,*,#2495,.F.);
#3143=ORIENTED_EDGE('',*,*,#2496,.F.);
#3144=ORIENTED_EDGE('',*,*,#2470,.T.);
#3145=ORIENTED_EDGE('',*,*,#2497,.T.);
#3146=ORIENTED_EDGE('',*,*,#2496,.T.);
#3147=ORIENTED_EDGE('',*,*,#2498,.F.);
#3148=ORIENTED_EDGE('',*,*,#2499,.F.);
#3149=ORIENTED_EDGE('',*,*,#2437,.T.);
#3150=ORIENTED_EDGE('',*,*,#2451,.T.);
#3151=ORIENTED_EDGE('',*,*,#2465,.T.);
#3152=ORIENTED_EDGE('',*,*,#2500,.T.);
#3153=ORIENTED_EDGE('',*,*,#2499,.T.);
#3154=ORIENTED_EDGE('',*,*,#2501,.F.);
#3155=ORIENTED_EDGE('',*,*,#2491,.F.);
#3156=ORIENTED_EDGE('',*,*,#2473,.T.);
#3157=ORIENTED_EDGE('',*,*,#2501,.T.);
#3158=ORIENTED_EDGE('',*,*,#2498,.T.);
#3159=ORIENTED_EDGE('',*,*,#2495,.T.);
#3160=ORIENTED_EDGE('',*,*,#2492,.T.);
#3161=ORIENTED_EDGE('',*,*,#2480,.T.);
#3162=ORIENTED_EDGE('',*,*,#2484,.T.);
#3163=ORIENTED_EDGE('',*,*,#2500,.F.);
#3164=ORIENTED_EDGE('',*,*,#2490,.F.);
#3165=ORIENTED_EDGE('',*,*,#2494,.F.);
#3166=ORIENTED_EDGE('',*,*,#2497,.F.);
#3167=ORIENTED_EDGE('',*,*,#2486,.T.);
#3168=ORIENTED_EDGE('',*,*,#2488,.T.);
#3169=ORIENTED_EDGE('',*,*,#2502,.F.);
#3170=ORIENTED_EDGE('',*,*,#2503,.T.);
#3171=ORIENTED_EDGE('',*,*,#2504,.T.);
#3172=ORIENTED_EDGE('',*,*,#2503,.F.);
#3173=ORIENTED_EDGE('',*,*,#2502,.T.);
#3174=ORIENTED_EDGE('',*,*,#2504,.F.);
#3175=ORIENTED_EDGE('',*,*,#2505,.F.);
#3176=ORIENTED_EDGE('',*,*,#2506,.T.);
#3177=ORIENTED_EDGE('',*,*,#2507,.F.);
#3178=ORIENTED_EDGE('',*,*,#2506,.F.);
#3179=ORIENTED_EDGE('',*,*,#2508,.F.);
#3180=ORIENTED_EDGE('',*,*,#2509,.T.);
#3181=ORIENTED_EDGE('',*,*,#2510,.F.);
#3182=ORIENTED_EDGE('',*,*,#2509,.F.);
#3183=ORIENTED_EDGE('',*,*,#2511,.T.);
#3184=ORIENTED_EDGE('',*,*,#2511,.F.);
#3185=ORIENTED_EDGE('',*,*,#2505,.T.);
#3186=ORIENTED_EDGE('',*,*,#2510,.T.);
#3187=ORIENTED_EDGE('',*,*,#2512,.F.);
#3188=ORIENTED_EDGE('',*,*,#2513,.T.);
#3189=ORIENTED_EDGE('',*,*,#2514,.F.);
#3190=ORIENTED_EDGE('',*,*,#2513,.F.);
#3191=ORIENTED_EDGE('',*,*,#2512,.T.);
#3192=ORIENTED_EDGE('',*,*,#2507,.T.);
#3193=ORIENTED_EDGE('',*,*,#2515,.F.);
#3194=ORIENTED_EDGE('',*,*,#2516,.T.);
#3195=ORIENTED_EDGE('',*,*,#2517,.T.);
#3196=ORIENTED_EDGE('',*,*,#2516,.F.);
#3197=ORIENTED_EDGE('',*,*,#2515,.T.);
#3198=ORIENTED_EDGE('',*,*,#2514,.T.);
#3199=ORIENTED_EDGE('',*,*,#2517,.F.);
#3200=ORIENTED_EDGE('',*,*,#2508,.T.);
#3201=ORIENTED_EDGE('',*,*,#2518,.F.);
#3202=ORIENTED_EDGE('',*,*,#2519,.T.);
#3203=ORIENTED_EDGE('',*,*,#2520,.F.);
#3204=ORIENTED_EDGE('',*,*,#2519,.F.);
#3205=ORIENTED_EDGE('',*,*,#2521,.F.);
#3206=ORIENTED_EDGE('',*,*,#2522,.T.);
#3207=ORIENTED_EDGE('',*,*,#2523,.F.);
#3208=ORIENTED_EDGE('',*,*,#2522,.F.);
#3209=ORIENTED_EDGE('',*,*,#2524,.T.);
#3210=ORIENTED_EDGE('',*,*,#2524,.F.);
#3211=ORIENTED_EDGE('',*,*,#2518,.T.);
#3212=ORIENTED_EDGE('',*,*,#2523,.T.);
#3213=ORIENTED_EDGE('',*,*,#2525,.F.);
#3214=ORIENTED_EDGE('',*,*,#2526,.T.);
#3215=ORIENTED_EDGE('',*,*,#2527,.F.);
#3216=ORIENTED_EDGE('',*,*,#2526,.F.);
#3217=ORIENTED_EDGE('',*,*,#2525,.T.);
#3218=ORIENTED_EDGE('',*,*,#2520,.T.);
#3219=ORIENTED_EDGE('',*,*,#2528,.F.);
#3220=ORIENTED_EDGE('',*,*,#2529,.T.);
#3221=ORIENTED_EDGE('',*,*,#2530,.T.);
#3222=ORIENTED_EDGE('',*,*,#2529,.F.);
#3223=ORIENTED_EDGE('',*,*,#2528,.T.);
#3224=ORIENTED_EDGE('',*,*,#2527,.T.);
#3225=ORIENTED_EDGE('',*,*,#2530,.F.);
#3226=ORIENTED_EDGE('',*,*,#2521,.T.);
#3227=ORIENTED_EDGE('',*,*,#2531,.F.);
#3228=ORIENTED_EDGE('',*,*,#2532,.T.);
#3229=ORIENTED_EDGE('',*,*,#2533,.F.);
#3230=ORIENTED_EDGE('',*,*,#2532,.F.);
#3231=ORIENTED_EDGE('',*,*,#2534,.F.);
#3232=ORIENTED_EDGE('',*,*,#2535,.T.);
#3233=ORIENTED_EDGE('',*,*,#2536,.F.);
#3234=ORIENTED_EDGE('',*,*,#2535,.F.);
#3235=ORIENTED_EDGE('',*,*,#2537,.T.);
#3236=ORIENTED_EDGE('',*,*,#2537,.F.);
#3237=ORIENTED_EDGE('',*,*,#2531,.T.);
#3238=ORIENTED_EDGE('',*,*,#2536,.T.);
#3239=ORIENTED_EDGE('',*,*,#2538,.F.);
#3240=ORIENTED_EDGE('',*,*,#2539,.T.);
#3241=ORIENTED_EDGE('',*,*,#2540,.F.);
#3242=ORIENTED_EDGE('',*,*,#2539,.F.);
#3243=ORIENTED_EDGE('',*,*,#2538,.T.);
#3244=ORIENTED_EDGE('',*,*,#2533,.T.);
#3245=ORIENTED_EDGE('',*,*,#2541,.F.);
#3246=ORIENTED_EDGE('',*,*,#2542,.T.);
#3247=ORIENTED_EDGE('',*,*,#2543,.T.);
#3248=ORIENTED_EDGE('',*,*,#2542,.F.);
#3249=ORIENTED_EDGE('',*,*,#2541,.T.);
#3250=ORIENTED_EDGE('',*,*,#2540,.T.);
#3251=ORIENTED_EDGE('',*,*,#2543,.F.);
#3252=ORIENTED_EDGE('',*,*,#2534,.T.);
#3253=ORIENTED_EDGE('',*,*,#2544,.F.);
#3254=ORIENTED_EDGE('',*,*,#2545,.T.);
#3255=ORIENTED_EDGE('',*,*,#2546,.F.);
#3256=ORIENTED_EDGE('',*,*,#2547,.F.);
#3257=ORIENTED_EDGE('',*,*,#2548,.F.);
#3258=ORIENTED_EDGE('',*,*,#2549,.T.);
#3259=ORIENTED_EDGE('',*,*,#2550,.F.);
#3260=ORIENTED_EDGE('',*,*,#2545,.F.);
#3261=ORIENTED_EDGE('',*,*,#2551,.F.);
#3262=ORIENTED_EDGE('',*,*,#2552,.T.);
#3263=ORIENTED_EDGE('',*,*,#2553,.F.);
#3264=ORIENTED_EDGE('',*,*,#2549,.F.);
#3265=ORIENTED_EDGE('',*,*,#2554,.F.);
#3266=ORIENTED_EDGE('',*,*,#2555,.T.);
#3267=ORIENTED_EDGE('',*,*,#2556,.F.);
#3268=ORIENTED_EDGE('',*,*,#2552,.F.);
#3269=ORIENTED_EDGE('',*,*,#2557,.F.);
#3270=ORIENTED_EDGE('',*,*,#2558,.T.);
#3271=ORIENTED_EDGE('',*,*,#2559,.F.);
#3272=ORIENTED_EDGE('',*,*,#2555,.F.);
#3273=ORIENTED_EDGE('',*,*,#2560,.F.);
#3274=ORIENTED_EDGE('',*,*,#2561,.T.);
#3275=ORIENTED_EDGE('',*,*,#2562,.F.);
#3276=ORIENTED_EDGE('',*,*,#2558,.F.);
#3277=ORIENTED_EDGE('',*,*,#2563,.F.);
#3278=ORIENTED_EDGE('',*,*,#2564,.T.);
#3279=ORIENTED_EDGE('',*,*,#2565,.F.);
#3280=ORIENTED_EDGE('',*,*,#2561,.F.);
#3281=ORIENTED_EDGE('',*,*,#2566,.F.);
#3282=ORIENTED_EDGE('',*,*,#2567,.T.);
#3283=ORIENTED_EDGE('',*,*,#2568,.F.);
#3284=ORIENTED_EDGE('',*,*,#2564,.F.);
#3285=ORIENTED_EDGE('',*,*,#2569,.F.);
#3286=ORIENTED_EDGE('',*,*,#2570,.F.);
#3287=ORIENTED_EDGE('',*,*,#2571,.F.);
#3288=ORIENTED_EDGE('',*,*,#2567,.F.);
#3289=ORIENTED_EDGE('',*,*,#2572,.F.);
#3290=ORIENTED_EDGE('',*,*,#2573,.T.);
#3291=ORIENTED_EDGE('',*,*,#2574,.F.);
#3292=ORIENTED_EDGE('',*,*,#2575,.F.);
#3293=ORIENTED_EDGE('',*,*,#2576,.F.);
#3294=ORIENTED_EDGE('',*,*,#2577,.T.);
#3295=ORIENTED_EDGE('',*,*,#2578,.F.);
#3296=ORIENTED_EDGE('',*,*,#2573,.F.);
#3297=ORIENTED_EDGE('',*,*,#2579,.F.);
#3298=ORIENTED_EDGE('',*,*,#2580,.T.);
#3299=ORIENTED_EDGE('',*,*,#2581,.F.);
#3300=ORIENTED_EDGE('',*,*,#2577,.F.);
#3301=ORIENTED_EDGE('',*,*,#2582,.F.);
#3302=ORIENTED_EDGE('',*,*,#2583,.T.);
#3303=ORIENTED_EDGE('',*,*,#2584,.F.);
#3304=ORIENTED_EDGE('',*,*,#2580,.F.);
#3305=ORIENTED_EDGE('',*,*,#2585,.F.);
#3306=ORIENTED_EDGE('',*,*,#2586,.T.);
#3307=ORIENTED_EDGE('',*,*,#2587,.F.);
#3308=ORIENTED_EDGE('',*,*,#2583,.F.);
#3309=ORIENTED_EDGE('',*,*,#2588,.F.);
#3310=ORIENTED_EDGE('',*,*,#2589,.T.);
#3311=ORIENTED_EDGE('',*,*,#2590,.F.);
#3312=ORIENTED_EDGE('',*,*,#2586,.F.);
#3313=ORIENTED_EDGE('',*,*,#2591,.F.);
#3314=ORIENTED_EDGE('',*,*,#2592,.T.);
#3315=ORIENTED_EDGE('',*,*,#2593,.F.);
#3316=ORIENTED_EDGE('',*,*,#2589,.F.);
#3317=ORIENTED_EDGE('',*,*,#2594,.F.);
#3318=ORIENTED_EDGE('',*,*,#2595,.T.);
#3319=ORIENTED_EDGE('',*,*,#2596,.F.);
#3320=ORIENTED_EDGE('',*,*,#2592,.F.);
#3321=ORIENTED_EDGE('',*,*,#2597,.F.);
#3322=ORIENTED_EDGE('',*,*,#2598,.F.);
#3323=ORIENTED_EDGE('',*,*,#2599,.F.);
#3324=ORIENTED_EDGE('',*,*,#2595,.F.);
#3325=ORIENTED_EDGE('',*,*,#2600,.F.);
#3326=ORIENTED_EDGE('',*,*,#2601,.T.);
#3327=ORIENTED_EDGE('',*,*,#2602,.F.);
#3328=ORIENTED_EDGE('',*,*,#2603,.F.);
#3329=ORIENTED_EDGE('',*,*,#2604,.F.);
#3330=ORIENTED_EDGE('',*,*,#2605,.T.);
#3331=ORIENTED_EDGE('',*,*,#2606,.F.);
#3332=ORIENTED_EDGE('',*,*,#2601,.F.);
#3333=ORIENTED_EDGE('',*,*,#2607,.F.);
#3334=ORIENTED_EDGE('',*,*,#2608,.T.);
#3335=ORIENTED_EDGE('',*,*,#2609,.F.);
#3336=ORIENTED_EDGE('',*,*,#2605,.F.);
#3337=ORIENTED_EDGE('',*,*,#2610,.F.);
#3338=ORIENTED_EDGE('',*,*,#2611,.T.);
#3339=ORIENTED_EDGE('',*,*,#2612,.F.);
#3340=ORIENTED_EDGE('',*,*,#2608,.F.);
#3341=ORIENTED_EDGE('',*,*,#2613,.F.);
#3342=ORIENTED_EDGE('',*,*,#2614,.T.);
#3343=ORIENTED_EDGE('',*,*,#2615,.F.);
#3344=ORIENTED_EDGE('',*,*,#2611,.F.);
#3345=ORIENTED_EDGE('',*,*,#2616,.F.);
#3346=ORIENTED_EDGE('',*,*,#2617,.T.);
#3347=ORIENTED_EDGE('',*,*,#2618,.F.);
#3348=ORIENTED_EDGE('',*,*,#2614,.F.);
#3349=ORIENTED_EDGE('',*,*,#2619,.F.);
#3350=ORIENTED_EDGE('',*,*,#2620,.T.);
#3351=ORIENTED_EDGE('',*,*,#2621,.F.);
#3352=ORIENTED_EDGE('',*,*,#2617,.F.);
#3353=ORIENTED_EDGE('',*,*,#2622,.F.);
#3354=ORIENTED_EDGE('',*,*,#2623,.T.);
#3355=ORIENTED_EDGE('',*,*,#2624,.F.);
#3356=ORIENTED_EDGE('',*,*,#2620,.F.);
#3357=ORIENTED_EDGE('',*,*,#2625,.F.);
#3358=ORIENTED_EDGE('',*,*,#2626,.F.);
#3359=ORIENTED_EDGE('',*,*,#2627,.F.);
#3360=ORIENTED_EDGE('',*,*,#2623,.F.);
#3361=ORIENTED_EDGE('',*,*,#2628,.F.);
#3362=ORIENTED_EDGE('',*,*,#2629,.T.);
#3363=ORIENTED_EDGE('',*,*,#2630,.F.);
#3364=ORIENTED_EDGE('',*,*,#2631,.F.);
#3365=ORIENTED_EDGE('',*,*,#2632,.F.);
#3366=ORIENTED_EDGE('',*,*,#2633,.T.);
#3367=ORIENTED_EDGE('',*,*,#2634,.F.);
#3368=ORIENTED_EDGE('',*,*,#2629,.F.);
#3369=ORIENTED_EDGE('',*,*,#2635,.F.);
#3370=ORIENTED_EDGE('',*,*,#2636,.T.);
#3371=ORIENTED_EDGE('',*,*,#2637,.F.);
#3372=ORIENTED_EDGE('',*,*,#2633,.F.);
#3373=ORIENTED_EDGE('',*,*,#2638,.F.);
#3374=ORIENTED_EDGE('',*,*,#2639,.T.);
#3375=ORIENTED_EDGE('',*,*,#2640,.F.);
#3376=ORIENTED_EDGE('',*,*,#2636,.F.);
#3377=ORIENTED_EDGE('',*,*,#2641,.F.);
#3378=ORIENTED_EDGE('',*,*,#2642,.T.);
#3379=ORIENTED_EDGE('',*,*,#2643,.F.);
#3380=ORIENTED_EDGE('',*,*,#2639,.F.);
#3381=ORIENTED_EDGE('',*,*,#2644,.F.);
#3382=ORIENTED_EDGE('',*,*,#2645,.T.);
#3383=ORIENTED_EDGE('',*,*,#2646,.F.);
#3384=ORIENTED_EDGE('',*,*,#2642,.F.);
#3385=ORIENTED_EDGE('',*,*,#2647,.F.);
#3386=ORIENTED_EDGE('',*,*,#2648,.T.);
#3387=ORIENTED_EDGE('',*,*,#2649,.F.);
#3388=ORIENTED_EDGE('',*,*,#2645,.F.);
#3389=ORIENTED_EDGE('',*,*,#2650,.F.);
#3390=ORIENTED_EDGE('',*,*,#2651,.T.);
#3391=ORIENTED_EDGE('',*,*,#2652,.F.);
#3392=ORIENTED_EDGE('',*,*,#2648,.F.);
#3393=ORIENTED_EDGE('',*,*,#2653,.F.);
#3394=ORIENTED_EDGE('',*,*,#2654,.F.);
#3395=ORIENTED_EDGE('',*,*,#2655,.F.);
#3396=ORIENTED_EDGE('',*,*,#2651,.F.);
#3397=ORIENTED_EDGE('',*,*,#2656,.F.);
#3398=ORIENTED_EDGE('',*,*,#2657,.T.);
#3399=ORIENTED_EDGE('',*,*,#2658,.F.);
#3400=ORIENTED_EDGE('',*,*,#2657,.F.);
#3401=ORIENTED_EDGE('',*,*,#2570,.T.);
#3402=ORIENTED_EDGE('',*,*,#2659,.T.);
#3403=ORIENTED_EDGE('',*,*,#2660,.T.);
#3404=ORIENTED_EDGE('',*,*,#2661,.F.);
#3405=ORIENTED_EDGE('',*,*,#2547,.T.);
#3406=ORIENTED_EDGE('',*,*,#2662,.F.);
#3407=ORIENTED_EDGE('',*,*,#2663,.F.);
#3408=ORIENTED_EDGE('',*,*,#2664,.T.);
#3409=ORIENTED_EDGE('',*,*,#2598,.T.);
#3410=ORIENTED_EDGE('',*,*,#2665,.T.);
#3411=ORIENTED_EDGE('',*,*,#2663,.T.);
#3412=ORIENTED_EDGE('',*,*,#2666,.F.);
#3413=ORIENTED_EDGE('',*,*,#2575,.T.);
#3414=ORIENTED_EDGE('',*,*,#2667,.F.);
#3415=ORIENTED_EDGE('',*,*,#2668,.F.);
#3416=ORIENTED_EDGE('',*,*,#2669,.T.);
#3417=ORIENTED_EDGE('',*,*,#2626,.T.);
#3418=ORIENTED_EDGE('',*,*,#2670,.T.);
#3419=ORIENTED_EDGE('',*,*,#2668,.T.);
#3420=ORIENTED_EDGE('',*,*,#2671,.F.);
#3421=ORIENTED_EDGE('',*,*,#2603,.T.);
#3422=ORIENTED_EDGE('',*,*,#2672,.F.);
#3423=ORIENTED_EDGE('',*,*,#2673,.F.);
#3424=ORIENTED_EDGE('',*,*,#2674,.T.);
#3425=ORIENTED_EDGE('',*,*,#2654,.T.);
#3426=ORIENTED_EDGE('',*,*,#2675,.T.);
#3427=ORIENTED_EDGE('',*,*,#2673,.T.);
#3428=ORIENTED_EDGE('',*,*,#2676,.F.);
#3429=ORIENTED_EDGE('',*,*,#2631,.T.);
#3430=ORIENTED_EDGE('',*,*,#2677,.F.);
#3431=ORIENTED_EDGE('',*,*,#2660,.F.);
#3432=ORIENTED_EDGE('',*,*,#2678,.T.);
#3433=ORIENTED_EDGE('',*,*,#2546,.T.);
#3434=ORIENTED_EDGE('',*,*,#2550,.T.);
#3435=ORIENTED_EDGE('',*,*,#2553,.T.);
#3436=ORIENTED_EDGE('',*,*,#2556,.T.);
#3437=ORIENTED_EDGE('',*,*,#2559,.T.);
#3438=ORIENTED_EDGE('',*,*,#2562,.T.);
#3439=ORIENTED_EDGE('',*,*,#2565,.T.);
#3440=ORIENTED_EDGE('',*,*,#2568,.T.);
#3441=ORIENTED_EDGE('',*,*,#2571,.T.);
#3442=ORIENTED_EDGE('',*,*,#2661,.T.);
#3443=ORIENTED_EDGE('',*,*,#2677,.T.);
#3444=ORIENTED_EDGE('',*,*,#2630,.T.);
#3445=ORIENTED_EDGE('',*,*,#2634,.T.);
#3446=ORIENTED_EDGE('',*,*,#2637,.T.);
#3447=ORIENTED_EDGE('',*,*,#2640,.T.);
#3448=ORIENTED_EDGE('',*,*,#2643,.T.);
#3449=ORIENTED_EDGE('',*,*,#2646,.T.);
#3450=ORIENTED_EDGE('',*,*,#2649,.T.);
#3451=ORIENTED_EDGE('',*,*,#2652,.T.);
#3452=ORIENTED_EDGE('',*,*,#2655,.T.);
#3453=ORIENTED_EDGE('',*,*,#2676,.T.);
#3454=ORIENTED_EDGE('',*,*,#2672,.T.);
#3455=ORIENTED_EDGE('',*,*,#2602,.T.);
#3456=ORIENTED_EDGE('',*,*,#2606,.T.);
#3457=ORIENTED_EDGE('',*,*,#2609,.T.);
#3458=ORIENTED_EDGE('',*,*,#2612,.T.);
#3459=ORIENTED_EDGE('',*,*,#2615,.T.);
#3460=ORIENTED_EDGE('',*,*,#2618,.T.);
#3461=ORIENTED_EDGE('',*,*,#2621,.T.);
#3462=ORIENTED_EDGE('',*,*,#2624,.T.);
#3463=ORIENTED_EDGE('',*,*,#2627,.T.);
#3464=ORIENTED_EDGE('',*,*,#2671,.T.);
#3465=ORIENTED_EDGE('',*,*,#2667,.T.);
#3466=ORIENTED_EDGE('',*,*,#2574,.T.);
#3467=ORIENTED_EDGE('',*,*,#2578,.T.);
#3468=ORIENTED_EDGE('',*,*,#2581,.T.);
#3469=ORIENTED_EDGE('',*,*,#2584,.T.);
#3470=ORIENTED_EDGE('',*,*,#2587,.T.);
#3471=ORIENTED_EDGE('',*,*,#2590,.T.);
#3472=ORIENTED_EDGE('',*,*,#2593,.T.);
#3473=ORIENTED_EDGE('',*,*,#2596,.T.);
#3474=ORIENTED_EDGE('',*,*,#2599,.T.);
#3475=ORIENTED_EDGE('',*,*,#2666,.T.);
#3476=ORIENTED_EDGE('',*,*,#2662,.T.);
#3477=ORIENTED_EDGE('',*,*,#2658,.T.);
#3478=ORIENTED_EDGE('',*,*,#2544,.T.);
#3479=ORIENTED_EDGE('',*,*,#2664,.F.);
#3480=ORIENTED_EDGE('',*,*,#2665,.F.);
#3481=ORIENTED_EDGE('',*,*,#2597,.T.);
#3482=ORIENTED_EDGE('',*,*,#2594,.T.);
#3483=ORIENTED_EDGE('',*,*,#2591,.T.);
#3484=ORIENTED_EDGE('',*,*,#2588,.T.);
#3485=ORIENTED_EDGE('',*,*,#2585,.T.);
#3486=ORIENTED_EDGE('',*,*,#2582,.T.);
#3487=ORIENTED_EDGE('',*,*,#2579,.T.);
#3488=ORIENTED_EDGE('',*,*,#2576,.T.);
#3489=ORIENTED_EDGE('',*,*,#2572,.T.);
#3490=ORIENTED_EDGE('',*,*,#2669,.F.);
#3491=ORIENTED_EDGE('',*,*,#2670,.F.);
#3492=ORIENTED_EDGE('',*,*,#2625,.T.);
#3493=ORIENTED_EDGE('',*,*,#2622,.T.);
#3494=ORIENTED_EDGE('',*,*,#2619,.T.);
#3495=ORIENTED_EDGE('',*,*,#2616,.T.);
#3496=ORIENTED_EDGE('',*,*,#2613,.T.);
#3497=ORIENTED_EDGE('',*,*,#2610,.T.);
#3498=ORIENTED_EDGE('',*,*,#2607,.T.);
#3499=ORIENTED_EDGE('',*,*,#2604,.T.);
#3500=ORIENTED_EDGE('',*,*,#2600,.T.);
#3501=ORIENTED_EDGE('',*,*,#2674,.F.);
#3502=ORIENTED_EDGE('',*,*,#2675,.F.);
#3503=ORIENTED_EDGE('',*,*,#2653,.T.);
#3504=ORIENTED_EDGE('',*,*,#2650,.T.);
#3505=ORIENTED_EDGE('',*,*,#2647,.T.);
#3506=ORIENTED_EDGE('',*,*,#2644,.T.);
#3507=ORIENTED_EDGE('',*,*,#2641,.T.);
#3508=ORIENTED_EDGE('',*,*,#2638,.T.);
#3509=ORIENTED_EDGE('',*,*,#2635,.T.);
#3510=ORIENTED_EDGE('',*,*,#2632,.T.);
#3511=ORIENTED_EDGE('',*,*,#2628,.T.);
#3512=ORIENTED_EDGE('',*,*,#2678,.F.);
#3513=ORIENTED_EDGE('',*,*,#2659,.F.);
#3514=ORIENTED_EDGE('',*,*,#2569,.T.);
#3515=ORIENTED_EDGE('',*,*,#2566,.T.);
#3516=ORIENTED_EDGE('',*,*,#2563,.T.);
#3517=ORIENTED_EDGE('',*,*,#2560,.T.);
#3518=ORIENTED_EDGE('',*,*,#2557,.T.);
#3519=ORIENTED_EDGE('',*,*,#2554,.T.);
#3520=ORIENTED_EDGE('',*,*,#2551,.T.);
#3521=ORIENTED_EDGE('',*,*,#2548,.T.);
#3522=ORIENTED_EDGE('',*,*,#2656,.T.);
#3523=ORIENTED_EDGE('',*,*,#2679,.T.);
#3524=ORIENTED_EDGE('',*,*,#2680,.T.);
#3525=ORIENTED_EDGE('',*,*,#2681,.T.);
#3526=ORIENTED_EDGE('',*,*,#2680,.F.);
#3527=ORIENTED_EDGE('',*,*,#2681,.F.);
#3528=ORIENTED_EDGE('',*,*,#2682,.T.);
#3529=ORIENTED_EDGE('',*,*,#2683,.T.);
#3530=ORIENTED_EDGE('',*,*,#2682,.F.);
#3531=ORIENTED_EDGE('',*,*,#2684,.T.);
#3532=ORIENTED_EDGE('',*,*,#2679,.F.);
#3533=ORIENTED_EDGE('',*,*,#2684,.F.);
#3534=ORIENTED_EDGE('',*,*,#2685,.T.);
#3535=ORIENTED_EDGE('',*,*,#2686,.T.);
#3536=ORIENTED_EDGE('',*,*,#2685,.F.);
#3537=ORIENTED_EDGE('',*,*,#2686,.F.);
#3538=ORIENTED_EDGE('',*,*,#2683,.F.);
#3539=ORIENTED_EDGE('',*,*,#2687,.T.);
#3540=ORIENTED_EDGE('',*,*,#2688,.T.);
#3541=ORIENTED_EDGE('',*,*,#2689,.T.);
#3542=ORIENTED_EDGE('',*,*,#2690,.F.);
#3543=ORIENTED_EDGE('',*,*,#2691,.T.);
#3544=ORIENTED_EDGE('',*,*,#2692,.T.);
#3545=ORIENTED_EDGE('',*,*,#2693,.T.);
#3546=ORIENTED_EDGE('',*,*,#2688,.F.);
#3547=ORIENTED_EDGE('',*,*,#2694,.T.);
#3548=ORIENTED_EDGE('',*,*,#2695,.T.);
#3549=ORIENTED_EDGE('',*,*,#2696,.T.);
#3550=ORIENTED_EDGE('',*,*,#2692,.F.);
#3551=ORIENTED_EDGE('',*,*,#2697,.T.);
#3552=ORIENTED_EDGE('',*,*,#2698,.T.);
#3553=ORIENTED_EDGE('',*,*,#2699,.T.);
#3554=ORIENTED_EDGE('',*,*,#2695,.F.);
#3555=ORIENTED_EDGE('',*,*,#2700,.T.);
#3556=ORIENTED_EDGE('',*,*,#2701,.T.);
#3557=ORIENTED_EDGE('',*,*,#2702,.T.);
#3558=ORIENTED_EDGE('',*,*,#2698,.F.);
#3559=ORIENTED_EDGE('',*,*,#2703,.T.);
#3560=ORIENTED_EDGE('',*,*,#2690,.T.);
#3561=ORIENTED_EDGE('',*,*,#2704,.T.);
#3562=ORIENTED_EDGE('',*,*,#2701,.F.);
#3563=ORIENTED_EDGE('',*,*,#2703,.F.);
#3564=ORIENTED_EDGE('',*,*,#2700,.F.);
#3565=ORIENTED_EDGE('',*,*,#2697,.F.);
#3566=ORIENTED_EDGE('',*,*,#2694,.F.);
#3567=ORIENTED_EDGE('',*,*,#2691,.F.);
#3568=ORIENTED_EDGE('',*,*,#2687,.F.);
#3569=ORIENTED_EDGE('',*,*,#2704,.F.);
#3570=ORIENTED_EDGE('',*,*,#2689,.F.);
#3571=ORIENTED_EDGE('',*,*,#2693,.F.);
#3572=ORIENTED_EDGE('',*,*,#2696,.F.);
#3573=ORIENTED_EDGE('',*,*,#2699,.F.);
#3574=ORIENTED_EDGE('',*,*,#2702,.F.);
#3575=ORIENTED_EDGE('',*,*,#2705,.F.);
#3576=ORIENTED_EDGE('',*,*,#2706,.F.);
#3577=ORIENTED_EDGE('',*,*,#2707,.F.);
#3578=ORIENTED_EDGE('',*,*,#2708,.T.);
#3579=ORIENTED_EDGE('',*,*,#2706,.T.);
#3580=ORIENTED_EDGE('',*,*,#2708,.F.);
#3581=ORIENTED_EDGE('',*,*,#2709,.F.);
#3582=ORIENTED_EDGE('',*,*,#2710,.T.);
#3583=ORIENTED_EDGE('',*,*,#2707,.T.);
#3584=ORIENTED_EDGE('',*,*,#2710,.F.);
#3585=ORIENTED_EDGE('',*,*,#2711,.F.);
#3586=ORIENTED_EDGE('',*,*,#2712,.T.);
#3587=ORIENTED_EDGE('',*,*,#2709,.T.);
#3588=ORIENTED_EDGE('',*,*,#2712,.F.);
#3589=ORIENTED_EDGE('',*,*,#2711,.T.);
#3590=ORIENTED_EDGE('',*,*,#2713,.F.);
#3591=ORIENTED_EDGE('',*,*,#2714,.F.);
#3592=ORIENTED_EDGE('',*,*,#2715,.T.);
#3593=ORIENTED_EDGE('',*,*,#2713,.T.);
#3594=ORIENTED_EDGE('',*,*,#2715,.F.);
#3595=ORIENTED_EDGE('',*,*,#2705,.T.);
#3596=ORIENTED_EDGE('',*,*,#2716,.T.);
#3597=ORIENTED_EDGE('',*,*,#2714,.T.);
#3598=ORIENTED_EDGE('',*,*,#2716,.F.);
#3599=ORIENTED_EDGE('',*,*,#2717,.F.);
#3600=ORIENTED_EDGE('',*,*,#2718,.F.);
#3601=ORIENTED_EDGE('',*,*,#2719,.T.);
#3602=ORIENTED_EDGE('',*,*,#2717,.T.);
#3603=ORIENTED_EDGE('',*,*,#2719,.F.);
#3604=ORIENTED_EDGE('',*,*,#2720,.F.);
#3605=ORIENTED_EDGE('',*,*,#2721,.T.);
#3606=ORIENTED_EDGE('',*,*,#2718,.T.);
#3607=ORIENTED_EDGE('',*,*,#2721,.F.);
#3608=ORIENTED_EDGE('',*,*,#2722,.F.);
#3609=ORIENTED_EDGE('',*,*,#2723,.T.);
#3610=ORIENTED_EDGE('',*,*,#2720,.T.);
#3611=ORIENTED_EDGE('',*,*,#2723,.F.);
#3612=ORIENTED_EDGE('',*,*,#2722,.T.);
#3613=ORIENTED_EDGE('',*,*,#2724,.F.);
#3614=ORIENTED_EDGE('',*,*,#2725,.F.);
#3615=ORIENTED_EDGE('',*,*,#2726,.T.);
#3616=ORIENTED_EDGE('',*,*,#2724,.T.);
#3617=ORIENTED_EDGE('',*,*,#2726,.F.);
#3618=ORIENTED_EDGE('',*,*,#2727,.F.);
#3619=ORIENTED_EDGE('',*,*,#2728,.T.);
#3620=ORIENTED_EDGE('',*,*,#2725,.T.);
#3621=ORIENTED_EDGE('',*,*,#2728,.F.);
#3622=ORIENTED_EDGE('',*,*,#2729,.F.);
#3623=ORIENTED_EDGE('',*,*,#2730,.T.);
#3624=ORIENTED_EDGE('',*,*,#2727,.T.);
#3625=ORIENTED_EDGE('',*,*,#2730,.F.);
#3626=ORIENTED_EDGE('',*,*,#2729,.T.);
#3627=ORIENTED_EDGE('',*,*,#2731,.T.);
#3628=ORIENTED_EDGE('',*,*,#2732,.T.);
#3629=ORIENTED_EDGE('',*,*,#2733,.T.);
#3630=ORIENTED_EDGE('',*,*,#2734,.F.);
#3631=ORIENTED_EDGE('',*,*,#2735,.T.);
#3632=ORIENTED_EDGE('',*,*,#2736,.T.);
#3633=ORIENTED_EDGE('',*,*,#2737,.T.);
#3634=ORIENTED_EDGE('',*,*,#2732,.F.);
#3635=ORIENTED_EDGE('',*,*,#2738,.T.);
#3636=ORIENTED_EDGE('',*,*,#2739,.T.);
#3637=ORIENTED_EDGE('',*,*,#2740,.T.);
#3638=ORIENTED_EDGE('',*,*,#2736,.F.);
#3639=ORIENTED_EDGE('',*,*,#2741,.T.);
#3640=ORIENTED_EDGE('',*,*,#2742,.T.);
#3641=ORIENTED_EDGE('',*,*,#2743,.T.);
#3642=ORIENTED_EDGE('',*,*,#2739,.F.);
#3643=ORIENTED_EDGE('',*,*,#2744,.T.);
#3644=ORIENTED_EDGE('',*,*,#2745,.T.);
#3645=ORIENTED_EDGE('',*,*,#2746,.T.);
#3646=ORIENTED_EDGE('',*,*,#2742,.F.);
#3647=ORIENTED_EDGE('',*,*,#2747,.T.);
#3648=ORIENTED_EDGE('',*,*,#2734,.T.);
#3649=ORIENTED_EDGE('',*,*,#2748,.T.);
#3650=ORIENTED_EDGE('',*,*,#2745,.F.);
#3651=ORIENTED_EDGE('',*,*,#2747,.F.);
#3652=ORIENTED_EDGE('',*,*,#2744,.F.);
#3653=ORIENTED_EDGE('',*,*,#2741,.F.);
#3654=ORIENTED_EDGE('',*,*,#2738,.F.);
#3655=ORIENTED_EDGE('',*,*,#2735,.F.);
#3656=ORIENTED_EDGE('',*,*,#2731,.F.);
#3657=ORIENTED_EDGE('',*,*,#2748,.F.);
#3658=ORIENTED_EDGE('',*,*,#2733,.F.);
#3659=ORIENTED_EDGE('',*,*,#2737,.F.);
#3660=ORIENTED_EDGE('',*,*,#2740,.F.);
#3661=ORIENTED_EDGE('',*,*,#2743,.F.);
#3662=ORIENTED_EDGE('',*,*,#2746,.F.);
#3663=ORIENTED_EDGE('',*,*,#2749,.T.);
#3664=ORIENTED_EDGE('',*,*,#2750,.T.);
#3665=ORIENTED_EDGE('',*,*,#2751,.T.);
#3666=ORIENTED_EDGE('',*,*,#2752,.T.);
#3667=ORIENTED_EDGE('',*,*,#2753,.T.);
#3668=ORIENTED_EDGE('',*,*,#2754,.T.);
#3669=ORIENTED_EDGE('',*,*,#2755,.F.);
#3670=ORIENTED_EDGE('',*,*,#2756,.T.);
#3671=ORIENTED_EDGE('',*,*,#2757,.T.);
#3672=ORIENTED_EDGE('',*,*,#2758,.T.);
#3673=ORIENTED_EDGE('',*,*,#2759,.T.);
#3674=ORIENTED_EDGE('',*,*,#2760,.T.);
#3675=ORIENTED_EDGE('',*,*,#2761,.T.);
#3676=ORIENTED_EDGE('',*,*,#2762,.F.);
#3677=ORIENTED_EDGE('',*,*,#2763,.F.);
#3678=ORIENTED_EDGE('',*,*,#2761,.F.);
#3679=ORIENTED_EDGE('',*,*,#2764,.F.);
#3680=ORIENTED_EDGE('',*,*,#2750,.F.);
#3681=ORIENTED_EDGE('',*,*,#2764,.T.);
#3682=ORIENTED_EDGE('',*,*,#2760,.F.);
#3683=ORIENTED_EDGE('',*,*,#2765,.F.);
#3684=ORIENTED_EDGE('',*,*,#2751,.F.);
#3685=ORIENTED_EDGE('',*,*,#2765,.T.);
#3686=ORIENTED_EDGE('',*,*,#2759,.F.);
#3687=ORIENTED_EDGE('',*,*,#2766,.F.);
#3688=ORIENTED_EDGE('',*,*,#2752,.F.);
#3689=ORIENTED_EDGE('',*,*,#2766,.T.);
#3690=ORIENTED_EDGE('',*,*,#2758,.F.);
#3691=ORIENTED_EDGE('',*,*,#2767,.F.);
#3692=ORIENTED_EDGE('',*,*,#2753,.F.);
#3693=ORIENTED_EDGE('',*,*,#2767,.T.);
#3694=ORIENTED_EDGE('',*,*,#2757,.F.);
#3695=ORIENTED_EDGE('',*,*,#2768,.F.);
#3696=ORIENTED_EDGE('',*,*,#2754,.F.);
#3697=ORIENTED_EDGE('',*,*,#2768,.T.);
#3698=ORIENTED_EDGE('',*,*,#2756,.F.);
#3699=ORIENTED_EDGE('',*,*,#2763,.T.);
#3700=ORIENTED_EDGE('',*,*,#2749,.F.);
#3701=ORIENTED_EDGE('',*,*,#2762,.T.);
#3702=ORIENTED_EDGE('',*,*,#2769,.T.);
#3703=ORIENTED_EDGE('',*,*,#2770,.T.);
#3704=ORIENTED_EDGE('',*,*,#2769,.F.);
#3705=ORIENTED_EDGE('',*,*,#2771,.F.);
#3706=ORIENTED_EDGE('',*,*,#2772,.T.);
#3707=ORIENTED_EDGE('',*,*,#2770,.F.);
#3708=ORIENTED_EDGE('',*,*,#2773,.T.);
#3709=ORIENTED_EDGE('',*,*,#2771,.T.);
#3710=ORIENTED_EDGE('',*,*,#2773,.F.);
#3711=ORIENTED_EDGE('',*,*,#2774,.F.);
#3712=ORIENTED_EDGE('',*,*,#2775,.T.);
#3713=ORIENTED_EDGE('',*,*,#2755,.T.);
#3714=ORIENTED_EDGE('',*,*,#2775,.F.);
#3715=ORIENTED_EDGE('',*,*,#2776,.F.);
#3716=ORIENTED_EDGE('',*,*,#2777,.T.);
#3717=ORIENTED_EDGE('',*,*,#2774,.T.);
#3718=ORIENTED_EDGE('',*,*,#2777,.F.);
#3719=ORIENTED_EDGE('',*,*,#2776,.T.);
#3720=ORIENTED_EDGE('',*,*,#2778,.F.);
#3721=ORIENTED_EDGE('',*,*,#2778,.T.);
#3722=ORIENTED_EDGE('',*,*,#2779,.T.);
#3723=ORIENTED_EDGE('',*,*,#2772,.F.);
#3724=ORIENTED_EDGE('',*,*,#2779,.F.);
#3725=ORIENTED_EDGE('',*,*,#2780,.F.);
#3726=ORIENTED_EDGE('',*,*,#2781,.T.);
#3727=ORIENTED_EDGE('',*,*,#2782,.T.);
#3728=ORIENTED_EDGE('',*,*,#2781,.F.);
#3729=ORIENTED_EDGE('',*,*,#2782,.F.);
#3730=ORIENTED_EDGE('',*,*,#2783,.F.);
#3731=ORIENTED_EDGE('',*,*,#2783,.T.);
#3732=ORIENTED_EDGE('',*,*,#2784,.T.);
#3733=ORIENTED_EDGE('',*,*,#2785,.F.);
#3734=ORIENTED_EDGE('',*,*,#2784,.F.);
#3735=ORIENTED_EDGE('',*,*,#2786,.F.);
#3736=ORIENTED_EDGE('',*,*,#2787,.T.);
#3737=ORIENTED_EDGE('',*,*,#2788,.T.);
#3738=ORIENTED_EDGE('',*,*,#2787,.F.);
#3739=ORIENTED_EDGE('',*,*,#2788,.F.);
#3740=ORIENTED_EDGE('',*,*,#2780,.T.);
#3741=ORIENTED_EDGE('',*,*,#2789,.T.);
#3742=ORIENTED_EDGE('',*,*,#2789,.F.);
#3743=ORIENTED_EDGE('',*,*,#2785,.T.);
#3744=ORIENTED_EDGE('',*,*,#2786,.T.);
#3745=ORIENTED_EDGE('',*,*,#2790,.F.);
#3746=ORIENTED_EDGE('',*,*,#2791,.T.);
#3747=ORIENTED_EDGE('',*,*,#2792,.T.);
#3748=ORIENTED_EDGE('',*,*,#2791,.F.);
#3749=ORIENTED_EDGE('',*,*,#2793,.F.);
#3750=ORIENTED_EDGE('',*,*,#2794,.T.);
#3751=ORIENTED_EDGE('',*,*,#2795,.T.);
#3752=ORIENTED_EDGE('',*,*,#2794,.F.);
#3753=ORIENTED_EDGE('',*,*,#2793,.T.);
#3754=ORIENTED_EDGE('',*,*,#2790,.T.);
#3755=ORIENTED_EDGE('',*,*,#2795,.F.);
#3756=ORIENTED_EDGE('',*,*,#2792,.F.);
#3757=ORIENTED_EDGE('',*,*,#2796,.F.);
#3758=ORIENTED_EDGE('',*,*,#2797,.T.);
#3759=ORIENTED_EDGE('',*,*,#2798,.F.);
#3760=ORIENTED_EDGE('',*,*,#2797,.F.);
#3761=ORIENTED_EDGE('',*,*,#2796,.T.);
#3762=ORIENTED_EDGE('',*,*,#2799,.F.);
#3763=ORIENTED_EDGE('',*,*,#2799,.T.);
#3764=ORIENTED_EDGE('',*,*,#2800,.T.);
#3765=ORIENTED_EDGE('',*,*,#2801,.T.);
#3766=ORIENTED_EDGE('',*,*,#2800,.F.);
#3767=ORIENTED_EDGE('',*,*,#2802,.F.);
#3768=ORIENTED_EDGE('',*,*,#2803,.T.);
#3769=ORIENTED_EDGE('',*,*,#2804,.T.);
#3770=ORIENTED_EDGE('',*,*,#2803,.F.);
#3771=ORIENTED_EDGE('',*,*,#2802,.T.);
#3772=ORIENTED_EDGE('',*,*,#2798,.T.);
#3773=ORIENTED_EDGE('',*,*,#2804,.F.);
#3774=ORIENTED_EDGE('',*,*,#2801,.F.);
#3775=ORIENTED_EDGE('',*,*,#2805,.F.);
#3776=ORIENTED_EDGE('',*,*,#2806,.T.);
#3777=ORIENTED_EDGE('',*,*,#2807,.T.);
#3778=ORIENTED_EDGE('',*,*,#2806,.F.);
#3779=ORIENTED_EDGE('',*,*,#2807,.F.);
#3780=ORIENTED_EDGE('',*,*,#2808,.F.);
#3781=ORIENTED_EDGE('',*,*,#2808,.T.);
#3782=ORIENTED_EDGE('',*,*,#2809,.T.);
#3783=ORIENTED_EDGE('',*,*,#2810,.F.);
#3784=ORIENTED_EDGE('',*,*,#2809,.F.);
#3785=ORIENTED_EDGE('',*,*,#2811,.F.);
#3786=ORIENTED_EDGE('',*,*,#2812,.T.);
#3787=ORIENTED_EDGE('',*,*,#2813,.T.);
#3788=ORIENTED_EDGE('',*,*,#2812,.F.);
#3789=ORIENTED_EDGE('',*,*,#2813,.F.);
#3790=ORIENTED_EDGE('',*,*,#2805,.T.);
#3791=ORIENTED_EDGE('',*,*,#2814,.T.);
#3792=ORIENTED_EDGE('',*,*,#2814,.F.);
#3793=ORIENTED_EDGE('',*,*,#2810,.T.);
#3794=ORIENTED_EDGE('',*,*,#2811,.T.);
#3795=ORIENTED_EDGE('',*,*,#2815,.F.);
#3796=ORIENTED_EDGE('',*,*,#2816,.T.);
#3797=ORIENTED_EDGE('',*,*,#2817,.T.);
#3798=ORIENTED_EDGE('',*,*,#2816,.F.);
#3799=ORIENTED_EDGE('',*,*,#2818,.F.);
#3800=ORIENTED_EDGE('',*,*,#2819,.T.);
#3801=ORIENTED_EDGE('',*,*,#2820,.T.);
#3802=ORIENTED_EDGE('',*,*,#2819,.F.);
#3803=ORIENTED_EDGE('',*,*,#2818,.T.);
#3804=ORIENTED_EDGE('',*,*,#2815,.T.);
#3805=ORIENTED_EDGE('',*,*,#2820,.F.);
#3806=ORIENTED_EDGE('',*,*,#2817,.F.);
#3807=ORIENTED_EDGE('',*,*,#2821,.F.);
#3808=ORIENTED_EDGE('',*,*,#2822,.T.);
#3809=ORIENTED_EDGE('',*,*,#2823,.F.);
#3810=ORIENTED_EDGE('',*,*,#2822,.F.);
#3811=ORIENTED_EDGE('',*,*,#2821,.T.);
#3812=ORIENTED_EDGE('',*,*,#2824,.F.);
#3813=ORIENTED_EDGE('',*,*,#2824,.T.);
#3814=ORIENTED_EDGE('',*,*,#2825,.T.);
#3815=ORIENTED_EDGE('',*,*,#2826,.T.);
#3816=ORIENTED_EDGE('',*,*,#2825,.F.);
#3817=ORIENTED_EDGE('',*,*,#2827,.F.);
#3818=ORIENTED_EDGE('',*,*,#2828,.T.);
#3819=ORIENTED_EDGE('',*,*,#2829,.T.);
#3820=ORIENTED_EDGE('',*,*,#2828,.F.);
#3821=ORIENTED_EDGE('',*,*,#2827,.T.);
#3822=ORIENTED_EDGE('',*,*,#2823,.T.);
#3823=ORIENTED_EDGE('',*,*,#2829,.F.);
#3824=ORIENTED_EDGE('',*,*,#2826,.F.);
#3825=ORIENTED_EDGE('',*,*,#2830,.F.);
#3826=ORIENTED_EDGE('',*,*,#2831,.T.);
#3827=ORIENTED_EDGE('',*,*,#2832,.T.);
#3828=ORIENTED_EDGE('',*,*,#2831,.F.);
#3829=ORIENTED_EDGE('',*,*,#2832,.F.);
#3830=ORIENTED_EDGE('',*,*,#2833,.F.);
#3831=ORIENTED_EDGE('',*,*,#2833,.T.);
#3832=ORIENTED_EDGE('',*,*,#2834,.T.);
#3833=ORIENTED_EDGE('',*,*,#2835,.F.);
#3834=ORIENTED_EDGE('',*,*,#2834,.F.);
#3835=ORIENTED_EDGE('',*,*,#2836,.F.);
#3836=ORIENTED_EDGE('',*,*,#2837,.T.);
#3837=ORIENTED_EDGE('',*,*,#2838,.T.);
#3838=ORIENTED_EDGE('',*,*,#2837,.F.);
#3839=ORIENTED_EDGE('',*,*,#2838,.F.);
#3840=ORIENTED_EDGE('',*,*,#2830,.T.);
#3841=ORIENTED_EDGE('',*,*,#2839,.T.);
#3842=ORIENTED_EDGE('',*,*,#2839,.F.);
#3843=ORIENTED_EDGE('',*,*,#2835,.T.);
#3844=ORIENTED_EDGE('',*,*,#2836,.T.);
#3845=ORIENTED_EDGE('',*,*,#2840,.F.);
#3846=ORIENTED_EDGE('',*,*,#2841,.T.);
#3847=ORIENTED_EDGE('',*,*,#2842,.T.);
#3848=ORIENTED_EDGE('',*,*,#2841,.F.);
#3849=ORIENTED_EDGE('',*,*,#2843,.F.);
#3850=ORIENTED_EDGE('',*,*,#2844,.T.);
#3851=ORIENTED_EDGE('',*,*,#2845,.T.);
#3852=ORIENTED_EDGE('',*,*,#2844,.F.);
#3853=ORIENTED_EDGE('',*,*,#2843,.T.);
#3854=ORIENTED_EDGE('',*,*,#2840,.T.);
#3855=ORIENTED_EDGE('',*,*,#2845,.F.);
#3856=ORIENTED_EDGE('',*,*,#2842,.F.);
#3857=ORIENTED_EDGE('',*,*,#2846,.F.);
#3858=ORIENTED_EDGE('',*,*,#2847,.T.);
#3859=ORIENTED_EDGE('',*,*,#2848,.F.);
#3860=ORIENTED_EDGE('',*,*,#2847,.F.);
#3861=ORIENTED_EDGE('',*,*,#2846,.T.);
#3862=ORIENTED_EDGE('',*,*,#2849,.F.);
#3863=ORIENTED_EDGE('',*,*,#2849,.T.);
#3864=ORIENTED_EDGE('',*,*,#2850,.T.);
#3865=ORIENTED_EDGE('',*,*,#2851,.T.);
#3866=ORIENTED_EDGE('',*,*,#2850,.F.);
#3867=ORIENTED_EDGE('',*,*,#2852,.F.);
#3868=ORIENTED_EDGE('',*,*,#2853,.T.);
#3869=ORIENTED_EDGE('',*,*,#2854,.T.);
#3870=ORIENTED_EDGE('',*,*,#2853,.F.);
#3871=ORIENTED_EDGE('',*,*,#2852,.T.);
#3872=ORIENTED_EDGE('',*,*,#2848,.T.);
#3873=ORIENTED_EDGE('',*,*,#2854,.F.);
#3874=ORIENTED_EDGE('',*,*,#2851,.F.);
#3875=ORIENTED_EDGE('',*,*,#2855,.F.);
#3876=ORIENTED_EDGE('',*,*,#2856,.T.);
#3877=ORIENTED_EDGE('',*,*,#2857,.F.);
#3878=ORIENTED_EDGE('',*,*,#2856,.F.);
#3879=ORIENTED_EDGE('',*,*,#2855,.T.);
#3880=ORIENTED_EDGE('',*,*,#2858,.F.);
#3881=ORIENTED_EDGE('',*,*,#2859,.T.);
#3882=ORIENTED_EDGE('',*,*,#2860,.T.);
#3883=ORIENTED_EDGE('',*,*,#2861,.T.);
#3884=ORIENTED_EDGE('',*,*,#2862,.T.);
#3885=ORIENTED_EDGE('',*,*,#2863,.T.);
#3886=ORIENTED_EDGE('',*,*,#2864,.T.);
#3887=ORIENTED_EDGE('',*,*,#2865,.T.);
#3888=ORIENTED_EDGE('',*,*,#2866,.F.);
#3889=ORIENTED_EDGE('',*,*,#2867,.F.);
#3890=ORIENTED_EDGE('',*,*,#2868,.F.);
#3891=ORIENTED_EDGE('',*,*,#2869,.F.);
#3892=ORIENTED_EDGE('',*,*,#2870,.F.);
#3893=ORIENTED_EDGE('',*,*,#2871,.F.);
#3894=ORIENTED_EDGE('',*,*,#2872,.F.);
#3895=ORIENTED_EDGE('',*,*,#2867,.T.);
#3896=ORIENTED_EDGE('',*,*,#2873,.T.);
#3897=ORIENTED_EDGE('',*,*,#2864,.F.);
#3898=ORIENTED_EDGE('',*,*,#2874,.F.);
#3899=ORIENTED_EDGE('',*,*,#2868,.T.);
#3900=ORIENTED_EDGE('',*,*,#2874,.T.);
#3901=ORIENTED_EDGE('',*,*,#2863,.F.);
#3902=ORIENTED_EDGE('',*,*,#2875,.F.);
#3903=ORIENTED_EDGE('',*,*,#2869,.T.);
#3904=ORIENTED_EDGE('',*,*,#2875,.T.);
#3905=ORIENTED_EDGE('',*,*,#2862,.F.);
#3906=ORIENTED_EDGE('',*,*,#2876,.F.);
#3907=ORIENTED_EDGE('',*,*,#2870,.T.);
#3908=ORIENTED_EDGE('',*,*,#2876,.T.);
#3909=ORIENTED_EDGE('',*,*,#2861,.F.);
#3910=ORIENTED_EDGE('',*,*,#2877,.F.);
#3911=ORIENTED_EDGE('',*,*,#2871,.T.);
#3912=ORIENTED_EDGE('',*,*,#2877,.T.);
#3913=ORIENTED_EDGE('',*,*,#2860,.F.);
#3914=ORIENTED_EDGE('',*,*,#2878,.F.);
#3915=ORIENTED_EDGE('',*,*,#2866,.T.);
#3916=ORIENTED_EDGE('',*,*,#2878,.T.);
#3917=ORIENTED_EDGE('',*,*,#2859,.F.);
#3918=ORIENTED_EDGE('',*,*,#2873,.F.);
#3919=ORIENTED_EDGE('',*,*,#2879,.F.);
#3920=ORIENTED_EDGE('',*,*,#2857,.T.);
#3921=ORIENTED_EDGE('',*,*,#2879,.T.);
#3922=ORIENTED_EDGE('',*,*,#2880,.T.);
#3923=ORIENTED_EDGE('',*,*,#2881,.F.);
#3924=ORIENTED_EDGE('',*,*,#2880,.F.);
#3925=ORIENTED_EDGE('',*,*,#2882,.F.);
#3926=ORIENTED_EDGE('',*,*,#2881,.T.);
#3927=ORIENTED_EDGE('',*,*,#2865,.F.);
#3928=ORIENTED_EDGE('',*,*,#2883,.T.);
#3929=ORIENTED_EDGE('',*,*,#2882,.T.);
#3930=ORIENTED_EDGE('',*,*,#2883,.F.);
#3931=ORIENTED_EDGE('',*,*,#2884,.F.);
#3932=ORIENTED_EDGE('',*,*,#2885,.T.);
#3933=ORIENTED_EDGE('',*,*,#2872,.T.);
#3934=ORIENTED_EDGE('',*,*,#2885,.F.);
#3935=ORIENTED_EDGE('',*,*,#2884,.T.);
#3936=ORIENTED_EDGE('',*,*,#2886,.F.);
#3937=ORIENTED_EDGE('',*,*,#2886,.T.);
#3938=ORIENTED_EDGE('',*,*,#2887,.T.);
#3939=ORIENTED_EDGE('',*,*,#2858,.T.);
#3940=ORIENTED_EDGE('',*,*,#2887,.F.);
#3941=ORIENTED_EDGE('',*,*,#2888,.F.);
#3942=ORIENTED_EDGE('',*,*,#2889,.T.);
#3943=ORIENTED_EDGE('',*,*,#2890,.F.);
#3944=ORIENTED_EDGE('',*,*,#2891,.T.);
#3945=ORIENTED_EDGE('',*,*,#2888,.T.);
#3946=ORIENTED_EDGE('',*,*,#2891,.F.);
#3947=ORIENTED_EDGE('',*,*,#2890,.T.);
#3948=ORIENTED_EDGE('',*,*,#2892,.F.);
#3949=ORIENTED_EDGE('',*,*,#2893,.F.);
#3950=ORIENTED_EDGE('',*,*,#2894,.T.);
#3951=ORIENTED_EDGE('',*,*,#2892,.T.);
#3952=ORIENTED_EDGE('',*,*,#2894,.F.);
#3953=ORIENTED_EDGE('',*,*,#2893,.T.);
#3954=ORIENTED_EDGE('',*,*,#2895,.F.);
#3955=ORIENTED_EDGE('',*,*,#2895,.T.);
#3956=ORIENTED_EDGE('',*,*,#2896,.T.);
#3957=ORIENTED_EDGE('',*,*,#2889,.F.);
#3958=ORIENTED_EDGE('',*,*,#2896,.F.);
#3959=CYLINDRICAL_SURFACE('',#4592,0.275);
#3960=CYLINDRICAL_SURFACE('',#4616,0.165);
#3961=CYLINDRICAL_SURFACE('',#4619,0.165);
#3962=CYLINDRICAL_SURFACE('',#4622,0.275);
#3963=CYLINDRICAL_SURFACE('',#4634,0.4);
#3964=CYLINDRICAL_SURFACE('',#4638,1.2);
#3965=CYLINDRICAL_SURFACE('',#4644,0.4);
#3966=CYLINDRICAL_SURFACE('',#4648,1.2);
#3967=CYLINDRICAL_SURFACE('',#4654,0.4);
#3968=CYLINDRICAL_SURFACE('',#4658,1.2);
#3969=CYLINDRICAL_SURFACE('',#4662,0.684999999999999);
#3970=CYLINDRICAL_SURFACE('',#4667,0.300000000000001);
#3971=CYLINDRICAL_SURFACE('',#4669,0.4);
#3972=CYLINDRICAL_SURFACE('',#4674,0.4);
#3973=CYLINDRICAL_SURFACE('',#4679,0.225);
#3974=CYLINDRICAL_SURFACE('',#4681,0.225);
#3975=CYLINDRICAL_SURFACE('',#4690,0.300000000000001);
#3976=CYLINDRICAL_SURFACE('',#4696,0.4);
#3977=CYLINDRICAL_SURFACE('',#4699,0.85);
#3978=CYLINDRICAL_SURFACE('',#4704,1.2);
#3979=CYLINDRICAL_SURFACE('',#4708,1.4);
#3980=CYLINDRICAL_SURFACE('',#4714,0.4);
#3981=CYLINDRICAL_SURFACE('',#4717,0.85);
#3982=CYLINDRICAL_SURFACE('',#4722,1.2);
#3983=CYLINDRICAL_SURFACE('',#4726,1.4);
#3984=CYLINDRICAL_SURFACE('',#4732,0.4);
#3985=CYLINDRICAL_SURFACE('',#4735,0.85);
#3986=CYLINDRICAL_SURFACE('',#4740,1.2);
#3987=CYLINDRICAL_SURFACE('',#4744,1.4);
#3988=CYLINDRICAL_SURFACE('',#4786,0.21);
#3989=CYLINDRICAL_SURFACE('',#4803,0.265);
#3990=CYLINDRICAL_SURFACE('',#4807,0.5);
#3991=CYLINDRICAL_SURFACE('',#4825,0.425);
#3992=CYLINDRICAL_SURFACE('',#4833,0.24505);
#3993=CYLINDRICAL_SURFACE('',#4839,0.35);
#3994=CYLINDRICAL_SURFACE('',#4847,0.1954);
#3995=CYLINDRICAL_SURFACE('',#4871,0.685);
#3996=CYLINDRICAL_SURFACE('',#4877,0.685);
#3997=CYLINDRICAL_SURFACE('',#4883,0.46);
#3998=CYLINDRICAL_SURFACE('',#4903,0.515);
#3999=CYLINDRICAL_SURFACE('',#4908,0.2);
#4000=CYLINDRICAL_SURFACE('',#4910,0.6);
#4001=CYLINDRICAL_SURFACE('',#4917,0.2);
#4002=CYLINDRICAL_SURFACE('',#4920,0.3);
#4003=CYLINDRICAL_SURFACE('',#4926,0.3);
#4004=CYLINDRICAL_SURFACE('',#4931,0.0750000000000002);
#4005=CYLINDRICAL_SURFACE('',#4933,0.4);
#4006=CYLINDRICAL_SURFACE('',#4940,0.515);
#4007=CYLINDRICAL_SURFACE('',#4945,0.2);
#4008=CYLINDRICAL_SURFACE('',#4947,0.6);
#4009=CYLINDRICAL_SURFACE('',#4954,0.2);
#4010=CYLINDRICAL_SURFACE('',#4957,0.3);
#4011=CYLINDRICAL_SURFACE('',#4963,0.3);
#4012=CYLINDRICAL_SURFACE('',#4968,0.075);
#4013=CYLINDRICAL_SURFACE('',#4970,0.4);
#4014=CYLINDRICAL_SURFACE('',#4977,0.515);
#4015=CYLINDRICAL_SURFACE('',#4982,0.2);
#4016=CYLINDRICAL_SURFACE('',#4984,0.6);
#4017=CYLINDRICAL_SURFACE('',#4991,0.2);
#4018=CYLINDRICAL_SURFACE('',#4994,0.3);
#4019=CYLINDRICAL_SURFACE('',#5000,0.3);
#4020=CYLINDRICAL_SURFACE('',#5005,0.0750000000000002);
#4021=CYLINDRICAL_SURFACE('',#5007,0.4);
#4022=CYLINDRICAL_SURFACE('',#5014,0.43);
#4023=CYLINDRICAL_SURFACE('',#5031,0.46);
#4024=CYLINDRICAL_SURFACE('',#5035,0.525);
#4025=CYLINDRICAL_SURFACE('',#5036,0.515);
#4026=CYLINDRICAL_SURFACE('',#5040,0.2);
#4027=CYLINDRICAL_SURFACE('',#5045,0.475);
#4028=CYLINDRICAL_SURFACE('',#5049,0.355);
#4029=CYLINDRICAL_SURFACE('',#5053,0.31);
#4030=ADVANCED_FACE('',(#540),#3959,.F.);
#4031=ADVANCED_FACE('',(#541),#371,.T.);
#4032=ADVANCED_FACE('',(#542),#372,.T.);
#4033=ADVANCED_FACE('',(#543),#373,.T.);
#4034=ADVANCED_FACE('',(#544),#374,.T.);
#4035=ADVANCED_FACE('',(#545,#285),#375,.T.);
#4036=ADVANCED_FACE('',(#546,#286),#376,.F.);
#4037=ADVANCED_FACE('',(#547),#377,.T.);
#4038=ADVANCED_FACE('',(#548),#378,.T.);
#4039=ADVANCED_FACE('',(#549),#379,.T.);
#4040=ADVANCED_FACE('',(#550),#380,.T.);
#4041=ADVANCED_FACE('',(#551),#381,.T.);
#4042=ADVANCED_FACE('',(#552),#382,.F.);
#4043=ADVANCED_FACE('',(#553),#383,.T.);
#4044=ADVANCED_FACE('',(#554),#384,.T.);
#4045=ADVANCED_FACE('',(#555),#385,.T.);
#4046=ADVANCED_FACE('',(#556),#386,.T.);
#4047=ADVANCED_FACE('',(#557),#387,.T.);
#4048=ADVANCED_FACE('',(#558),#388,.F.);
#4049=ADVANCED_FACE('',(#559),#3960,.F.);
#4050=ADVANCED_FACE('',(#560),#3961,.F.);
#4051=ADVANCED_FACE('',(#561),#3962,.F.);
#4052=ADVANCED_FACE('',(#562),#389,.T.);
#4053=ADVANCED_FACE('',(#563),#390,.T.);
#4054=ADVANCED_FACE('',(#564),#391,.T.);
#4055=ADVANCED_FACE('',(#565),#392,.T.);
#4056=ADVANCED_FACE('',(#566,#287,#288,#289),#393,.T.);
#4057=ADVANCED_FACE('',(#567,#290,#291,#292),#394,.F.);
#4058=ADVANCED_FACE('',(#568),#395,.F.);
#4059=ADVANCED_FACE('',(#569),#3963,.F.);
#4060=ADVANCED_FACE('',(#570),#396,.F.);
#4061=ADVANCED_FACE('',(#571),#3964,.F.);
#4062=ADVANCED_FACE('',(#572,#293),#397,.F.);
#4063=ADVANCED_FACE('',(#573),#398,.F.);
#4064=ADVANCED_FACE('',(#574),#3965,.F.);
#4065=ADVANCED_FACE('',(#575),#399,.F.);
#4066=ADVANCED_FACE('',(#576),#3966,.F.);
#4067=ADVANCED_FACE('',(#577,#294),#400,.F.);
#4068=ADVANCED_FACE('',(#578),#401,.F.);
#4069=ADVANCED_FACE('',(#579),#3967,.F.);
#4070=ADVANCED_FACE('',(#580),#402,.F.);
#4071=ADVANCED_FACE('',(#581),#3968,.F.);
#4072=ADVANCED_FACE('',(#582,#295),#403,.F.);
#4073=ADVANCED_FACE('',(#583,#296),#3969,.F.);
#4074=ADVANCED_FACE('',(#584,#297),#404,.T.);
#4075=ADVANCED_FACE('',(#585),#3970,.F.);
#4076=ADVANCED_FACE('',(#586),#3971,.F.);
#4077=ADVANCED_FACE('',(#587,#298),#405,.T.);
#4078=ADVANCED_FACE('',(#588,#299),#3972,.F.);
#4079=ADVANCED_FACE('',(#589,#300),#406,.T.);
#4080=ADVANCED_FACE('',(#590),#3973,.F.);
#4081=ADVANCED_FACE('',(#591),#3974,.F.);
#4082=ADVANCED_FACE('',(#592),#407,.T.);
#4083=ADVANCED_FACE('',(#593,#301),#408,.T.);
#4084=ADVANCED_FACE('',(#594,#302,#303,#304),#409,.T.);
#4085=ADVANCED_FACE('',(#595,#305),#410,.T.);
#4086=ADVANCED_FACE('',(#596,#306,#307),#411,.T.);
#4087=ADVANCED_FACE('',(#597,#308,#309),#412,.F.);
#4088=ADVANCED_FACE('',(#598),#3975,.T.);
#4089=ADVANCED_FACE('',(#599),#413,.T.);
#4090=ADVANCED_FACE('',(#600),#414,.F.);
#4091=ADVANCED_FACE('',(#601),#3976,.F.);
#4092=ADVANCED_FACE('',(#602),#3977,.F.);
#4093=ADVANCED_FACE('',(#603,#310,#311),#165,.F.);
#4094=ADVANCED_FACE('',(#604),#3978,.T.);
#4095=ADVANCED_FACE('',(#605,#312),#415,.T.);
#4096=ADVANCED_FACE('',(#606),#3979,.T.);
#4097=ADVANCED_FACE('',(#607,#313),#416,.T.);
#4098=ADVANCED_FACE('',(#608,#314),#417,.F.);
#4099=ADVANCED_FACE('',(#609),#3980,.F.);
#4100=ADVANCED_FACE('',(#610),#3981,.F.);
#4101=ADVANCED_FACE('',(#611,#315,#316),#166,.F.);
#4102=ADVANCED_FACE('',(#612),#3982,.T.);
#4103=ADVANCED_FACE('',(#613,#317),#418,.T.);
#4104=ADVANCED_FACE('',(#614),#3983,.T.);
#4105=ADVANCED_FACE('',(#615,#318),#419,.T.);
#4106=ADVANCED_FACE('',(#616,#319),#420,.F.);
#4107=ADVANCED_FACE('',(#617),#3984,.F.);
#4108=ADVANCED_FACE('',(#618),#3985,.F.);
#4109=ADVANCED_FACE('',(#619,#320,#321),#167,.F.);
#4110=ADVANCED_FACE('',(#620),#3986,.T.);
#4111=ADVANCED_FACE('',(#621,#322),#421,.T.);
#4112=ADVANCED_FACE('',(#622),#3987,.T.);
#4113=ADVANCED_FACE('',(#623,#323),#422,.T.);
#4114=ADVANCED_FACE('',(#624,#324),#423,.F.);
#4115=ADVANCED_FACE('',(#625),#424,.F.);
#4116=ADVANCED_FACE('',(#626),#425,.F.);
#4117=ADVANCED_FACE('',(#627),#426,.F.);
#4118=ADVANCED_FACE('',(#628),#427,.F.);
#4119=ADVANCED_FACE('',(#629),#428,.F.);
#4120=ADVANCED_FACE('',(#630),#429,.F.);
#4121=ADVANCED_FACE('',(#631),#430,.F.);
#4122=ADVANCED_FACE('',(#632),#431,.F.);
#4123=ADVANCED_FACE('',(#633),#432,.F.);
#4124=ADVANCED_FACE('',(#634),#433,.F.);
#4125=ADVANCED_FACE('',(#635),#434,.F.);
#4126=ADVANCED_FACE('',(#636),#435,.F.);
#4127=ADVANCED_FACE('',(#637),#436,.F.);
#4128=ADVANCED_FACE('',(#638),#437,.F.);
#4129=ADVANCED_FACE('',(#639),#438,.F.);
#4130=ADVANCED_FACE('',(#640),#439,.F.);
#4131=ADVANCED_FACE('',(#641),#440,.F.);
#4132=ADVANCED_FACE('',(#642),#441,.F.);
#4133=ADVANCED_FACE('',(#643),#442,.F.);
#4134=ADVANCED_FACE('',(#644),#443,.F.);
#4135=ADVANCED_FACE('',(#645),#444,.F.);
#4136=ADVANCED_FACE('',(#646),#445,.F.);
#4137=ADVANCED_FACE('',(#647),#446,.F.);
#4138=ADVANCED_FACE('',(#648),#447,.F.);
#4139=ADVANCED_FACE('',(#649),#448,.F.);
#4140=ADVANCED_FACE('',(#650),#449,.F.);
#4141=ADVANCED_FACE('',(#651),#450,.F.);
#4142=ADVANCED_FACE('',(#652),#451,.F.);
#4143=ADVANCED_FACE('',(#653),#452,.F.);
#4144=ADVANCED_FACE('',(#654),#453,.F.);
#4145=ADVANCED_FACE('',(#655),#454,.F.);
#4146=ADVANCED_FACE('',(#656),#455,.F.);
#4147=ADVANCED_FACE('',(#657),#456,.F.);
#4148=ADVANCED_FACE('',(#658),#457,.F.);
#4149=ADVANCED_FACE('',(#659),#458,.F.);
#4150=ADVANCED_FACE('',(#660),#459,.F.);
#4151=ADVANCED_FACE('',(#661),#3988,.F.);
#4152=ADVANCED_FACE('',(#662),#460,.T.);
#4153=ADVANCED_FACE('',(#663),#461,.T.);
#4154=ADVANCED_FACE('',(#664),#462,.T.);
#4155=ADVANCED_FACE('',(#665),#463,.T.);
#4156=ADVANCED_FACE('',(#666),#464,.T.);
#4157=ADVANCED_FACE('',(#667),#465,.T.);
#4158=ADVANCED_FACE('',(#668),#466,.T.);
#4159=ADVANCED_FACE('',(#669),#467,.T.);
#4160=ADVANCED_FACE('',(#670,#325),#468,.T.);
#4161=ADVANCED_FACE('',(#671,#326),#469,.F.);
#4162=ADVANCED_FACE('',(#672),#155,.F.);
#4163=ADVANCED_FACE('',(#673),#3989,.F.);
#4164=ADVANCED_FACE('',(#674,#327),#470,.T.);
#4165=ADVANCED_FACE('',(#675),#3990,.T.);
#4166=ADVANCED_FACE('',(#676,#328),#471,.F.);
#4167=ADVANCED_FACE('',(#677),#472,.F.);
#4168=ADVANCED_FACE('',(#678),#473,.F.);
#4169=ADVANCED_FACE('',(#679),#474,.F.);
#4170=ADVANCED_FACE('',(#680),#475,.F.);
#4171=ADVANCED_FACE('',(#681),#476,.F.);
#4172=ADVANCED_FACE('',(#682),#477,.F.);
#4173=ADVANCED_FACE('',(#683),#478,.F.);
#4174=ADVANCED_FACE('',(#684),#479,.F.);
#4175=ADVANCED_FACE('',(#685),#480,.F.);
#4176=ADVANCED_FACE('',(#686),#481,.T.);
#4177=ADVANCED_FACE('',(#687),#156,.T.);
#4178=ADVANCED_FACE('',(#688),#3991,.T.);
#4179=ADVANCED_FACE('',(#689),#157,.T.);
#4180=ADVANCED_FACE('',(#690,#329),#482,.T.);
#4181=ADVANCED_FACE('',(#691),#158,.T.);
#4182=ADVANCED_FACE('',(#692),#3992,.T.);
#4183=ADVANCED_FACE('',(#693),#483,.T.);
#4184=ADVANCED_FACE('',(#694),#159,.T.);
#4185=ADVANCED_FACE('',(#695),#3993,.T.);
#4186=ADVANCED_FACE('',(#696),#160,.T.);
#4187=ADVANCED_FACE('',(#697,#330),#484,.T.);
#4188=ADVANCED_FACE('',(#698),#161,.T.);
#4189=ADVANCED_FACE('',(#699),#3994,.T.);
#4190=ADVANCED_FACE('',(#700),#162,.T.);
#4191=ADVANCED_FACE('',(#701),#485,.T.);
#4192=ADVANCED_FACE('',(#702),#486,.F.);
#4193=ADVANCED_FACE('',(#703),#487,.F.);
#4194=ADVANCED_FACE('',(#704),#488,.F.);
#4195=ADVANCED_FACE('',(#705),#489,.F.);
#4196=ADVANCED_FACE('',(#706),#490,.F.);
#4197=ADVANCED_FACE('',(#707),#491,.F.);
#4198=ADVANCED_FACE('',(#708),#492,.F.);
#4199=ADVANCED_FACE('',(#709),#493,.F.);
#4200=ADVANCED_FACE('',(#710,#331),#494,.F.);
#4201=ADVANCED_FACE('',(#711,#332),#495,.T.);
#4202=ADVANCED_FACE('',(#712),#496,.T.);
#4203=ADVANCED_FACE('',(#713),#497,.T.);
#4204=ADVANCED_FACE('',(#714),#498,.T.);
#4205=ADVANCED_FACE('',(#715),#499,.T.);
#4206=ADVANCED_FACE('',(#716),#500,.T.);
#4207=ADVANCED_FACE('',(#717),#501,.T.);
#4208=ADVANCED_FACE('',(#718),#3995,.T.);
#4209=ADVANCED_FACE('',(#719,#333),#502,.T.);
#4210=ADVANCED_FACE('',(#720),#163,.T.);
#4211=ADVANCED_FACE('',(#721),#3996,.T.);
#4212=ADVANCED_FACE('',(#722),#164,.T.);
#4213=ADVANCED_FACE('',(#723,#334),#503,.T.);
#4214=ADVANCED_FACE('',(#724),#3997,.F.);
#4215=ADVANCED_FACE('',(#725),#3998,.F.);
#4216=ADVANCED_FACE('',(#726,#335),#504,.F.);
#4217=ADVANCED_FACE('',(#727),#3999,.F.);
#4218=ADVANCED_FACE('',(#728),#4000,.T.);
#4219=ADVANCED_FACE('',(#729,#336),#505,.F.);
#4220=ADVANCED_FACE('',(#730,#337,#338),#168,.T.);
#4221=ADVANCED_FACE('',(#731),#4001,.F.);
#4222=ADVANCED_FACE('',(#732),#4002,.T.);
#4223=ADVANCED_FACE('',(#733,#339),#506,.T.);
#4224=ADVANCED_FACE('',(#734,#340),#507,.F.);
#4225=ADVANCED_FACE('',(#735),#4003,.F.);
#4226=ADVANCED_FACE('',(#736,#341),#508,.T.);
#4227=ADVANCED_FACE('',(#737),#4004,.F.);
#4228=ADVANCED_FACE('',(#738),#4005,.T.);
#4229=ADVANCED_FACE('',(#739,#342),#509,.T.);
#4230=ADVANCED_FACE('',(#740,#343),#510,.F.);
#4231=ADVANCED_FACE('',(#741),#4006,.F.);
#4232=ADVANCED_FACE('',(#742,#344),#511,.F.);
#4233=ADVANCED_FACE('',(#743),#4007,.F.);
#4234=ADVANCED_FACE('',(#744),#4008,.T.);
#4235=ADVANCED_FACE('',(#745,#345),#512,.F.);
#4236=ADVANCED_FACE('',(#746,#346,#347),#169,.T.);
#4237=ADVANCED_FACE('',(#747),#4009,.F.);
#4238=ADVANCED_FACE('',(#748),#4010,.T.);
#4239=ADVANCED_FACE('',(#749,#348),#513,.T.);
#4240=ADVANCED_FACE('',(#750,#349),#514,.F.);
#4241=ADVANCED_FACE('',(#751),#4011,.F.);
#4242=ADVANCED_FACE('',(#752,#350),#515,.T.);
#4243=ADVANCED_FACE('',(#753),#4012,.F.);
#4244=ADVANCED_FACE('',(#754),#4013,.T.);
#4245=ADVANCED_FACE('',(#755,#351),#516,.T.);
#4246=ADVANCED_FACE('',(#756,#352),#517,.F.);
#4247=ADVANCED_FACE('',(#757),#4014,.F.);
#4248=ADVANCED_FACE('',(#758,#353),#518,.F.);
#4249=ADVANCED_FACE('',(#759),#4015,.F.);
#4250=ADVANCED_FACE('',(#760),#4016,.T.);
#4251=ADVANCED_FACE('',(#761,#354),#519,.F.);
#4252=ADVANCED_FACE('',(#762,#355,#356),#170,.T.);
#4253=ADVANCED_FACE('',(#763),#4017,.F.);
#4254=ADVANCED_FACE('',(#764),#4018,.T.);
#4255=ADVANCED_FACE('',(#765,#357),#520,.T.);
#4256=ADVANCED_FACE('',(#766,#358),#521,.F.);
#4257=ADVANCED_FACE('',(#767),#4019,.F.);
#4258=ADVANCED_FACE('',(#768,#359),#522,.T.);
#4259=ADVANCED_FACE('',(#769),#4020,.F.);
#4260=ADVANCED_FACE('',(#770),#4021,.T.);
#4261=ADVANCED_FACE('',(#771,#360),#523,.T.);
#4262=ADVANCED_FACE('',(#772,#361),#524,.F.);
#4263=ADVANCED_FACE('',(#773),#4022,.F.);
#4264=ADVANCED_FACE('',(#774,#362),#525,.T.);
#4265=ADVANCED_FACE('',(#775,#363),#526,.T.);
#4266=ADVANCED_FACE('',(#776,#364),#527,.F.);
#4267=ADVANCED_FACE('',(#777),#528,.T.);
#4268=ADVANCED_FACE('',(#778),#529,.T.);
#4269=ADVANCED_FACE('',(#779),#530,.T.);
#4270=ADVANCED_FACE('',(#780),#531,.T.);
#4271=ADVANCED_FACE('',(#781),#532,.T.);
#4272=ADVANCED_FACE('',(#782),#533,.T.);
#4273=ADVANCED_FACE('',(#783,#365),#534,.T.);
#4274=ADVANCED_FACE('',(#784),#4023,.F.);
#4275=ADVANCED_FACE('',(#785,#366),#535,.T.);
#4276=ADVANCED_FACE('',(#786),#4024,.T.);
#4277=ADVANCED_FACE('',(#787),#4025,.T.);
#4278=ADVANCED_FACE('',(#788,#367),#536,.T.);
#4279=ADVANCED_FACE('',(#789),#4026,.F.);
#4280=ADVANCED_FACE('',(#790,#368),#537,.T.);
#4281=ADVANCED_FACE('',(#791),#4027,.T.);
#4282=ADVANCED_FACE('',(#792,#369),#538,.T.);
#4283=ADVANCED_FACE('',(#793),#4028,.T.);
#4284=ADVANCED_FACE('',(#794,#370),#539,.T.);
#4285=ADVANCED_FACE('',(#795),#4029,.F.);
#4286=CLOSED_SHELL('',(#4030,#4031,#4032,#4033,#4034,#4035,#4036));
#4287=CLOSED_SHELL('',(#4037,#4038,#4039,#4040,#4041,#4042));
#4288=CLOSED_SHELL('',(#4043,#4044,#4045,#4046,#4047,#4048));
#4289=CLOSED_SHELL('',(#4049,#4050,#4051,#4052,#4053,#4054,#4055,#4056,
#4057));
#4290=CLOSED_SHELL('',(#4058,#4059,#4060,#4061,#4062,#4063,#4064,#4065,
#4066,#4067,#4068,#4069,#4070,#4071,#4072,#4073,#4074,#4075,#4076,#4077,
#4078,#4079,#4080,#4081,#4082,#4083,#4084,#4085,#4086,#4087));
#4291=CLOSED_SHELL('',(#4088,#4089,#4090));
#4292=CLOSED_SHELL('',(#4091,#4092,#4093,#4094,#4095,#4096,#4097,#4098));
#4293=CLOSED_SHELL('',(#4099,#4100,#4101,#4102,#4103,#4104,#4105,#4106));
#4294=CLOSED_SHELL('',(#4107,#4108,#4109,#4110,#4111,#4112,#4113,#4114));
#4295=CLOSED_SHELL('',(#4115,#4116,#4117,#4118,#4119,#4120,#4121,#4122,
#4123,#4124,#4125,#4126,#4127,#4128,#4129,#4130,#4131,#4132,#4133,#4134,
#4135,#4136,#4137,#4138,#4139,#4140,#4141,#4142,#4143,#4144,#4145,#4146,
#4147,#4148,#4149,#4150,#4151,#4152,#4153,#4154,#4155,#4156,#4157,#4158,
#4159,#4160,#4161));
#4296=CLOSED_SHELL('',(#4162,#4163,#4164,#4165,#4166));
#4297=CLOSED_SHELL('',(#4167,#4168,#4169,#4170,#4171,#4172,#4173,#4174));
#4298=CLOSED_SHELL('',(#4175,#4176,#4177,#4178,#4179,#4180,#4181,#4182));
#4299=CLOSED_SHELL('',(#4183,#4184,#4185,#4186,#4187,#4188,#4189,#4190,
#4191));
#4300=CLOSED_SHELL('',(#4192,#4193,#4194,#4195,#4196,#4197,#4198,#4199));
#4301=CLOSED_SHELL('',(#4200,#4201,#4202,#4203,#4204,#4205,#4206,#4207,
#4208,#4209,#4210,#4211,#4212,#4213,#4214));
#4302=CLOSED_SHELL('',(#4215,#4216,#4217,#4218,#4219,#4220));
#4303=CLOSED_SHELL('',(#4221,#4222,#4223,#4224));
#4304=CLOSED_SHELL('',(#4225,#4226,#4227,#4228,#4229,#4230));
#4305=CLOSED_SHELL('',(#4231,#4232,#4233,#4234,#4235,#4236));
#4306=CLOSED_SHELL('',(#4237,#4238,#4239,#4240));
#4307=CLOSED_SHELL('',(#4241,#4242,#4243,#4244,#4245,#4246));
#4308=CLOSED_SHELL('',(#4247,#4248,#4249,#4250,#4251,#4252));
#4309=CLOSED_SHELL('',(#4253,#4254,#4255,#4256));
#4310=CLOSED_SHELL('',(#4257,#4258,#4259,#4260,#4261,#4262));
#4311=CLOSED_SHELL('',(#4263,#4264,#4265,#4266,#4267,#4268,#4269,#4270,
#4271,#4272,#4273,#4274,#4275,#4276,#4277,#4278,#4279));
#4312=CLOSED_SHELL('',(#4280,#4281,#4282,#4283,#4284,#4285));
#4313=DERIVED_UNIT_ELEMENT(#4363,1.);
#4314=DERIVED_UNIT_ELEMENT(#7899,-3.);
#4315=DERIVED_UNIT_ELEMENT(#4363,1.);
#4316=DERIVED_UNIT_ELEMENT(#7899,-3.);
#4317=DERIVED_UNIT_ELEMENT(#4363,1.);
#4318=DERIVED_UNIT_ELEMENT(#7899,-3.);
#4319=DERIVED_UNIT_ELEMENT(#4363,1.);
#4320=DERIVED_UNIT_ELEMENT(#7899,-3.);
#4321=DERIVED_UNIT_ELEMENT(#4363,1.);
#4322=DERIVED_UNIT_ELEMENT(#7899,-3.);
#4323=DERIVED_UNIT_ELEMENT(#4363,1.);
#4324=DERIVED_UNIT_ELEMENT(#7899,-3.);
#4325=DERIVED_UNIT_ELEMENT(#4363,1.);
#4326=DERIVED_UNIT_ELEMENT(#7899,-3.);
#4327=DERIVED_UNIT_ELEMENT(#4363,1.);
#4328=DERIVED_UNIT_ELEMENT(#7899,-3.);
#4329=DERIVED_UNIT_ELEMENT(#4363,1.);
#4330=DERIVED_UNIT_ELEMENT(#7899,-3.);
#4331=DERIVED_UNIT_ELEMENT(#4363,1.);
#4332=DERIVED_UNIT_ELEMENT(#7899,-3.);
#4333=DERIVED_UNIT_ELEMENT(#4363,1.);
#4334=DERIVED_UNIT_ELEMENT(#7899,-3.);
#4335=DERIVED_UNIT_ELEMENT(#4363,1.);
#4336=DERIVED_UNIT_ELEMENT(#7899,-3.);
#4337=DERIVED_UNIT_ELEMENT(#4363,1.);
#4338=DERIVED_UNIT_ELEMENT(#7899,-3.);
#4339=DERIVED_UNIT_ELEMENT(#4363,1.);
#4340=DERIVED_UNIT_ELEMENT(#7899,-3.);
#4341=DERIVED_UNIT_ELEMENT(#4363,1.);
#4342=DERIVED_UNIT_ELEMENT(#7899,-3.);
#4343=DERIVED_UNIT_ELEMENT(#4363,1.);
#4344=DERIVED_UNIT_ELEMENT(#7899,-3.);
#4345=DERIVED_UNIT_ELEMENT(#4363,1.);
#4346=DERIVED_UNIT_ELEMENT(#7899,-3.);
#4347=DERIVED_UNIT_ELEMENT(#4363,1.);
#4348=DERIVED_UNIT_ELEMENT(#7899,-3.);
#4349=DERIVED_UNIT_ELEMENT(#4363,1.);
#4350=DERIVED_UNIT_ELEMENT(#7899,-3.);
#4351=DERIVED_UNIT_ELEMENT(#4363,1.);
#4352=DERIVED_UNIT_ELEMENT(#7899,-3.);
#4353=DERIVED_UNIT_ELEMENT(#4363,1.);
#4354=DERIVED_UNIT_ELEMENT(#7899,-3.);
#4355=DERIVED_UNIT_ELEMENT(#4363,1.);
#4356=DERIVED_UNIT_ELEMENT(#7899,-3.);
#4357=DERIVED_UNIT_ELEMENT(#4363,1.);
#4358=DERIVED_UNIT_ELEMENT(#7899,-3.);
#4359=DERIVED_UNIT_ELEMENT(#4363,1.);
#4360=DERIVED_UNIT_ELEMENT(#7899,-3.);
#4361=DERIVED_UNIT_ELEMENT(#4363,1.);
#4362=DERIVED_UNIT_ELEMENT(#7899,-3.);
#4363=(
MASS_UNIT()
NAMED_UNIT(*)
SI_UNIT(.KILO.,.GRAM.)
);
#4364=DERIVED_UNIT((#4313,#4314));
#4365=DERIVED_UNIT((#4315,#4316));
#4366=DERIVED_UNIT((#4317,#4318));
#4367=DERIVED_UNIT((#4319,#4320));
#4368=DERIVED_UNIT((#4321,#4322));
#4369=DERIVED_UNIT((#4323,#4324));
#4370=DERIVED_UNIT((#4325,#4326));
#4371=DERIVED_UNIT((#4327,#4328));
#4372=DERIVED_UNIT((#4329,#4330));
#4373=DERIVED_UNIT((#4331,#4332));
#4374=DERIVED_UNIT((#4333,#4334));
#4375=DERIVED_UNIT((#4335,#4336));
#4376=DERIVED_UNIT((#4337,#4338));
#4377=DERIVED_UNIT((#4339,#4340));
#4378=DERIVED_UNIT((#4341,#4342));
#4379=DERIVED_UNIT((#4343,#4344));
#4380=DERIVED_UNIT((#4345,#4346));
#4381=DERIVED_UNIT((#4347,#4348));
#4382=DERIVED_UNIT((#4349,#4350));
#4383=DERIVED_UNIT((#4351,#4352));
#4384=DERIVED_UNIT((#4353,#4354));
#4385=DERIVED_UNIT((#4355,#4356));
#4386=DERIVED_UNIT((#4357,#4358));
#4387=DERIVED_UNIT((#4359,#4360));
#4388=DERIVED_UNIT((#4361,#4362));
#4389=MEASURE_REPRESENTATION_ITEM('density measure',
POSITIVE_RATIO_MEASURE(7850.),#4364);
#4390=MEASURE_REPRESENTATION_ITEM('density measure',
POSITIVE_RATIO_MEASURE(7850.),#4365);
#4391=MEASURE_REPRESENTATION_ITEM('density measure',
POSITIVE_RATIO_MEASURE(7850.),#4366);
#4392=MEASURE_REPRESENTATION_ITEM('density measure',
POSITIVE_RATIO_MEASURE(7850.),#4367);
#4393=MEASURE_REPRESENTATION_ITEM('density measure',
POSITIVE_RATIO_MEASURE(7850.),#4368);
#4394=MEASURE_REPRESENTATION_ITEM('density measure',
POSITIVE_RATIO_MEASURE(7850.),#4369);
#4395=MEASURE_REPRESENTATION_ITEM('density measure',
POSITIVE_RATIO_MEASURE(7850.),#4370);
#4396=MEASURE_REPRESENTATION_ITEM('density measure',
POSITIVE_RATIO_MEASURE(7850.),#4371);
#4397=MEASURE_REPRESENTATION_ITEM('density measure',
POSITIVE_RATIO_MEASURE(7850.),#4372);
#4398=MEASURE_REPRESENTATION_ITEM('density measure',
POSITIVE_RATIO_MEASURE(7850.),#4373);
#4399=MEASURE_REPRESENTATION_ITEM('density measure',
POSITIVE_RATIO_MEASURE(7850.),#4374);
#4400=MEASURE_REPRESENTATION_ITEM('density measure',
POSITIVE_RATIO_MEASURE(7850.),#4375);
#4401=MEASURE_REPRESENTATION_ITEM('density measure',
POSITIVE_RATIO_MEASURE(7850.),#4376);
#4402=MEASURE_REPRESENTATION_ITEM('density measure',
POSITIVE_RATIO_MEASURE(7850.),#4377);
#4403=MEASURE_REPRESENTATION_ITEM('density measure',
POSITIVE_RATIO_MEASURE(7850.),#4378);
#4404=MEASURE_REPRESENTATION_ITEM('density measure',
POSITIVE_RATIO_MEASURE(7850.),#4379);
#4405=MEASURE_REPRESENTATION_ITEM('density measure',
POSITIVE_RATIO_MEASURE(7850.),#4380);
#4406=MEASURE_REPRESENTATION_ITEM('density measure',
POSITIVE_RATIO_MEASURE(7850.),#4381);
#4407=MEASURE_REPRESENTATION_ITEM('density measure',
POSITIVE_RATIO_MEASURE(7850.),#4382);
#4408=MEASURE_REPRESENTATION_ITEM('density measure',
POSITIVE_RATIO_MEASURE(7850.),#4383);
#4409=MEASURE_REPRESENTATION_ITEM('density measure',
POSITIVE_RATIO_MEASURE(7850.),#4384);
#4410=MEASURE_REPRESENTATION_ITEM('density measure',
POSITIVE_RATIO_MEASURE(7850.),#4385);
#4411=MEASURE_REPRESENTATION_ITEM('density measure',
POSITIVE_RATIO_MEASURE(7850.),#4386);
#4412=MEASURE_REPRESENTATION_ITEM('density measure',
POSITIVE_RATIO_MEASURE(7850.),#4387);
#4413=MEASURE_REPRESENTATION_ITEM('density measure',
POSITIVE_RATIO_MEASURE(7850.),#4388);
#4414=PROPERTY_DEFINITION_REPRESENTATION(#4539,#4464);
#4415=PROPERTY_DEFINITION_REPRESENTATION(#4540,#4465);
#4416=PROPERTY_DEFINITION_REPRESENTATION(#4541,#4466);
#4417=PROPERTY_DEFINITION_REPRESENTATION(#4542,#4467);
#4418=PROPERTY_DEFINITION_REPRESENTATION(#4543,#4468);
#4419=PROPERTY_DEFINITION_REPRESENTATION(#4544,#4469);
#4420=PROPERTY_DEFINITION_REPRESENTATION(#4545,#4470);
#4421=PROPERTY_DEFINITION_REPRESENTATION(#4546,#4471);
#4422=PROPERTY_DEFINITION_REPRESENTATION(#4547,#4472);
#4423=PROPERTY_DEFINITION_REPRESENTATION(#4548,#4473);
#4424=PROPERTY_DEFINITION_REPRESENTATION(#4549,#4474);
#4425=PROPERTY_DEFINITION_REPRESENTATION(#4550,#4475);
#4426=PROPERTY_DEFINITION_REPRESENTATION(#4551,#4476);
#4427=PROPERTY_DEFINITION_REPRESENTATION(#4552,#4477);
#4428=PROPERTY_DEFINITION_REPRESENTATION(#4553,#4478);
#4429=PROPERTY_DEFINITION_REPRESENTATION(#4554,#4479);
#4430=PROPERTY_DEFINITION_REPRESENTATION(#4555,#4480);
#4431=PROPERTY_DEFINITION_REPRESENTATION(#4556,#4481);
#4432=PROPERTY_DEFINITION_REPRESENTATION(#4557,#4482);
#4433=PROPERTY_DEFINITION_REPRESENTATION(#4558,#4483);
#4434=PROPERTY_DEFINITION_REPRESENTATION(#4559,#4484);
#4435=PROPERTY_DEFINITION_REPRESENTATION(#4560,#4485);
#4436=PROPERTY_DEFINITION_REPRESENTATION(#4561,#4486);
#4437=PROPERTY_DEFINITION_REPRESENTATION(#4562,#4487);
#4438=PROPERTY_DEFINITION_REPRESENTATION(#4563,#4488);
#4439=PROPERTY_DEFINITION_REPRESENTATION(#4564,#4489);
#4440=PROPERTY_DEFINITION_REPRESENTATION(#4565,#4490);
#4441=PROPERTY_DEFINITION_REPRESENTATION(#4566,#4491);
#4442=PROPERTY_DEFINITION_REPRESENTATION(#4567,#4492);
#4443=PROPERTY_DEFINITION_REPRESENTATION(#4568,#4493);
#4444=PROPERTY_DEFINITION_REPRESENTATION(#4569,#4494);
#4445=PROPERTY_DEFINITION_REPRESENTATION(#4570,#4495);
#4446=PROPERTY_DEFINITION_REPRESENTATION(#4571,#4496);
#4447=PROPERTY_DEFINITION_REPRESENTATION(#4572,#4497);
#4448=PROPERTY_DEFINITION_REPRESENTATION(#4573,#4498);
#4449=PROPERTY_DEFINITION_REPRESENTATION(#4574,#4499);
#4450=PROPERTY_DEFINITION_REPRESENTATION(#4575,#4500);
#4451=PROPERTY_DEFINITION_REPRESENTATION(#4576,#4501);
#4452=PROPERTY_DEFINITION_REPRESENTATION(#4577,#4502);
#4453=PROPERTY_DEFINITION_REPRESENTATION(#4578,#4503);
#4454=PROPERTY_DEFINITION_REPRESENTATION(#4579,#4504);
#4455=PROPERTY_DEFINITION_REPRESENTATION(#4580,#4505);
#4456=PROPERTY_DEFINITION_REPRESENTATION(#4581,#4506);
#4457=PROPERTY_DEFINITION_REPRESENTATION(#4582,#4507);
#4458=PROPERTY_DEFINITION_REPRESENTATION(#4583,#4508);
#4459=PROPERTY_DEFINITION_REPRESENTATION(#4584,#4509);
#4460=PROPERTY_DEFINITION_REPRESENTATION(#4585,#4510);
#4461=PROPERTY_DEFINITION_REPRESENTATION(#4586,#4511);
#4462=PROPERTY_DEFINITION_REPRESENTATION(#4587,#4512);
#4463=PROPERTY_DEFINITION_REPRESENTATION(#4588,#4513);
#4464=REPRESENTATION('material name',(#4514),#7868);
#4465=REPRESENTATION('density',(#4389),#7868);
#4466=REPRESENTATION('material name',(#4515),#7869);
#4467=REPRESENTATION('density',(#4390),#7869);
#4468=REPRESENTATION('material name',(#4516),#7870);
#4469=REPRESENTATION('density',(#4391),#7870);
#4470=REPRESENTATION('material name',(#4517),#7871);
#4471=REPRESENTATION('density',(#4392),#7871);
#4472=REPRESENTATION('material name',(#4518),#7872);
#4473=REPRESENTATION('density',(#4393),#7872);
#4474=REPRESENTATION('material name',(#4519),#7873);
#4475=REPRESENTATION('density',(#4394),#7873);
#4476=REPRESENTATION('material name',(#4520),#7874);
#4477=REPRESENTATION('density',(#4395),#7874);
#4478=REPRESENTATION('material name',(#4521),#7875);
#4479=REPRESENTATION('density',(#4396),#7875);
#4480=REPRESENTATION('material name',(#4522),#7876);
#4481=REPRESENTATION('density',(#4397),#7876);
#4482=REPRESENTATION('material name',(#4523),#7877);
#4483=REPRESENTATION('density',(#4398),#7877);
#4484=REPRESENTATION('material name',(#4524),#7878);
#4485=REPRESENTATION('density',(#4399),#7878);
#4486=REPRESENTATION('material name',(#4525),#7879);
#4487=REPRESENTATION('density',(#4400),#7879);
#4488=REPRESENTATION('material name',(#4526),#7880);
#4489=REPRESENTATION('density',(#4401),#7880);
#4490=REPRESENTATION('material name',(#4527),#7881);
#4491=REPRESENTATION('density',(#4402),#7881);
#4492=REPRESENTATION('material name',(#4528),#7883);
#4493=REPRESENTATION('density',(#4403),#7883);
#4494=REPRESENTATION('material name',(#4529),#7884);
#4495=REPRESENTATION('density',(#4404),#7884);
#4496=REPRESENTATION('material name',(#4530),#7885);
#4497=REPRESENTATION('density',(#4405),#7885);
#4498=REPRESENTATION('material name',(#4531),#7887);
#4499=REPRESENTATION('density',(#4406),#7887);
#4500=REPRESENTATION('material name',(#4532),#7888);
#4501=REPRESENTATION('density',(#4407),#7888);
#4502=REPRESENTATION('material name',(#4533),#7889);
#4503=REPRESENTATION('density',(#4408),#7889);
#4504=REPRESENTATION('material name',(#4534),#7891);
#4505=REPRESENTATION('density',(#4409),#7891);
#4506=REPRESENTATION('material name',(#4535),#7892);
#4507=REPRESENTATION('density',(#4410),#7892);
#4508=REPRESENTATION('material name',(#4536),#7893);
#4509=REPRESENTATION('density',(#4411),#7893);
#4510=REPRESENTATION('material name',(#4537),#7895);
#4511=REPRESENTATION('density',(#4412),#7895);
#4512=REPRESENTATION('material name',(#4538),#7896);
#4513=REPRESENTATION('density',(#4413),#7896);
#4514=DESCRIPTIVE_REPRESENTATION_ITEM('Steel','Steel');
#4515=DESCRIPTIVE_REPRESENTATION_ITEM('Steel','Steel');
#4516=DESCRIPTIVE_REPRESENTATION_ITEM('Steel','Steel');
#4517=DESCRIPTIVE_REPRESENTATION_ITEM('Steel','Steel');
#4518=DESCRIPTIVE_REPRESENTATION_ITEM('Steel','Steel');
#4519=DESCRIPTIVE_REPRESENTATION_ITEM('Steel','Steel');
#4520=DESCRIPTIVE_REPRESENTATION_ITEM('Steel','Steel');
#4521=DESCRIPTIVE_REPRESENTATION_ITEM('Steel','Steel');
#4522=DESCRIPTIVE_REPRESENTATION_ITEM('Steel','Steel');
#4523=DESCRIPTIVE_REPRESENTATION_ITEM('Steel','Steel');
#4524=DESCRIPTIVE_REPRESENTATION_ITEM('Steel','Steel');
#4525=DESCRIPTIVE_REPRESENTATION_ITEM('Steel','Steel');
#4526=DESCRIPTIVE_REPRESENTATION_ITEM('Steel','Steel');
#4527=DESCRIPTIVE_REPRESENTATION_ITEM('Steel','Steel');
#4528=DESCRIPTIVE_REPRESENTATION_ITEM('Steel','Steel');
#4529=DESCRIPTIVE_REPRESENTATION_ITEM('Steel','Steel');
#4530=DESCRIPTIVE_REPRESENTATION_ITEM('Steel','Steel');
#4531=DESCRIPTIVE_REPRESENTATION_ITEM('Steel','Steel');
#4532=DESCRIPTIVE_REPRESENTATION_ITEM('Steel','Steel');
#4533=DESCRIPTIVE_REPRESENTATION_ITEM('Steel','Steel');
#4534=DESCRIPTIVE_REPRESENTATION_ITEM('Steel','Steel');
#4535=DESCRIPTIVE_REPRESENTATION_ITEM('Steel','Steel');
#4536=DESCRIPTIVE_REPRESENTATION_ITEM('Steel','Steel');
#4537=DESCRIPTIVE_REPRESENTATION_ITEM('Steel','Steel');
#4538=DESCRIPTIVE_REPRESENTATION_ITEM('Steel','Steel');
#4539=PROPERTY_DEFINITION('material property','material name',#8033);
#4540=PROPERTY_DEFINITION('material property','density of part',#8033);
#4541=PROPERTY_DEFINITION('material property','material name',#8034);
#4542=PROPERTY_DEFINITION('material property','density of part',#8034);
#4543=PROPERTY_DEFINITION('material property','material name',#8035);
#4544=PROPERTY_DEFINITION('material property','density of part',#8035);
#4545=PROPERTY_DEFINITION('material property','material name',#8036);
#4546=PROPERTY_DEFINITION('material property','density of part',#8036);
#4547=PROPERTY_DEFINITION('material property','material name',#8037);
#4548=PROPERTY_DEFINITION('material property','density of part',#8037);
#4549=PROPERTY_DEFINITION('material property','material name',#8038);
#4550=PROPERTY_DEFINITION('material property','density of part',#8038);
#4551=PROPERTY_DEFINITION('material property','material name',#8039);
#4552=PROPERTY_DEFINITION('material property','density of part',#8039);
#4553=PROPERTY_DEFINITION('material property','material name',#8040);
#4554=PROPERTY_DEFINITION('material property','density of part',#8040);
#4555=PROPERTY_DEFINITION('material property','material name',#8041);
#4556=PROPERTY_DEFINITION('material property','density of part',#8041);
#4557=PROPERTY_DEFINITION('material property','material name',#8042);
#4558=PROPERTY_DEFINITION('material property','density of part',#8042);
#4559=PROPERTY_DEFINITION('material property','material name',#8043);
#4560=PROPERTY_DEFINITION('material property','density of part',#8043);
#4561=PROPERTY_DEFINITION('material property','material name',#8044);
#4562=PROPERTY_DEFINITION('material property','density of part',#8044);
#4563=PROPERTY_DEFINITION('material property','material name',#8045);
#4564=PROPERTY_DEFINITION('material property','density of part',#8045);
#4565=PROPERTY_DEFINITION('material property','material name',#8046);
#4566=PROPERTY_DEFINITION('material property','density of part',#8046);
#4567=PROPERTY_DEFINITION('material property','material name',#8048);
#4568=PROPERTY_DEFINITION('material property','density of part',#8048);
#4569=PROPERTY_DEFINITION('material property','material name',#8049);
#4570=PROPERTY_DEFINITION('material property','density of part',#8049);
#4571=PROPERTY_DEFINITION('material property','material name',#8050);
#4572=PROPERTY_DEFINITION('material property','density of part',#8050);
#4573=PROPERTY_DEFINITION('material property','material name',#8052);
#4574=PROPERTY_DEFINITION('material property','density of part',#8052);
#4575=PROPERTY_DEFINITION('material property','material name',#8053);
#4576=PROPERTY_DEFINITION('material property','density of part',#8053);
#4577=PROPERTY_DEFINITION('material property','material name',#8054);
#4578=PROPERTY_DEFINITION('material property','density of part',#8054);
#4579=PROPERTY_DEFINITION('material property','material name',#8056);
#4580=PROPERTY_DEFINITION('material property','density of part',#8056);
#4581=PROPERTY_DEFINITION('material property','material name',#8057);
#4582=PROPERTY_DEFINITION('material property','density of part',#8057);
#4583=PROPERTY_DEFINITION('material property','material name',#8058);
#4584=PROPERTY_DEFINITION('material property','density of part',#8058);
#4585=PROPERTY_DEFINITION('material property','material name',#8060);
#4586=PROPERTY_DEFINITION('material property','density of part',#8060);
#4587=PROPERTY_DEFINITION('material property','material name',#8061);
#4588=PROPERTY_DEFINITION('material property','density of part',#8061);
#4589=AXIS2_PLACEMENT_3D('',#6392,#5072,#5073);
#4590=AXIS2_PLACEMENT_3D('',#6393,#5074,#5075);
#4591=AXIS2_PLACEMENT_3D('',#6394,#5076,#5077);
#4592=AXIS2_PLACEMENT_3D('',#6395,#5078,#5079);
#4593=AXIS2_PLACEMENT_3D('',#6397,#5080,#5081);
#4594=AXIS2_PLACEMENT_3D('',#6400,#5083,#5084);
#4595=AXIS2_PLACEMENT_3D('',#6401,#5085,#5086);
#4596=AXIS2_PLACEMENT_3D('',#6410,#5091,#5092);
#4597=AXIS2_PLACEMENT_3D('',#6416,#5096,#5097);
#4598=AXIS2_PLACEMENT_3D('',#6422,#5101,#5102);
#4599=AXIS2_PLACEMENT_3D('',#6425,#5105,#5106);
#4600=AXIS2_PLACEMENT_3D('',#6426,#5107,#5108);
#4601=AXIS2_PLACEMENT_3D('',#6427,#5109,#5110);
#4602=AXIS2_PLACEMENT_3D('',#6428,#5111,#5112);
#4603=AXIS2_PLACEMENT_3D('',#6437,#5117,#5118);
#4604=AXIS2_PLACEMENT_3D('',#6443,#5122,#5123);
#4605=AXIS2_PLACEMENT_3D('',#6449,#5127,#5128);
#4606=AXIS2_PLACEMENT_3D('',#6452,#5131,#5132);
#4607=AXIS2_PLACEMENT_3D('',#6453,#5133,#5134);
#4608=AXIS2_PLACEMENT_3D('',#6454,#5135,#5136);
#4609=AXIS2_PLACEMENT_3D('',#6455,#5137,#5138);
#4610=AXIS2_PLACEMENT_3D('',#6464,#5143,#5144);
#4611=AXIS2_PLACEMENT_3D('',#6470,#5148,#5149);
#4612=AXIS2_PLACEMENT_3D('',#6476,#5153,#5154);
#4613=AXIS2_PLACEMENT_3D('',#6479,#5157,#5158);
#4614=AXIS2_PLACEMENT_3D('',#6480,#5159,#5160);
#4615=AXIS2_PLACEMENT_3D('',#6481,#5161,#5162);
#4616=AXIS2_PLACEMENT_3D('',#6482,#5163,#5164);
#4617=AXIS2_PLACEMENT_3D('',#6484,#5165,#5166);
#4618=AXIS2_PLACEMENT_3D('',#6487,#5168,#5169);
#4619=AXIS2_PLACEMENT_3D('',#6488,#5170,#5171);
#4620=AXIS2_PLACEMENT_3D('',#6490,#5172,#5173);
#4621=AXIS2_PLACEMENT_3D('',#6493,#5175,#5176);
#4622=AXIS2_PLACEMENT_3D('',#6494,#5177,#5178);
#4623=AXIS2_PLACEMENT_3D('',#6496,#5179,#5180);
#4624=AXIS2_PLACEMENT_3D('',#6499,#5182,#5183);
#4625=AXIS2_PLACEMENT_3D('',#6500,#5184,#5185);
#4626=AXIS2_PLACEMENT_3D('',#6509,#5190,#5191);
#4627=AXIS2_PLACEMENT_3D('',#6515,#5195,#5196);
#4628=AXIS2_PLACEMENT_3D('',#6521,#5200,#5201);
#4629=AXIS2_PLACEMENT_3D('',#6524,#5204,#5205);
#4630=AXIS2_PLACEMENT_3D('',#6525,#5206,#5207);
#4631=AXIS2_PLACEMENT_3D('',#6526,#5208,#5209);
#4632=AXIS2_PLACEMENT_3D('',#6527,#5210,#5211);
#4633=AXIS2_PLACEMENT_3D('',#6531,#5213,#5214);
#4634=AXIS2_PLACEMENT_3D('',#6532,#5215,#5216);
#4635=AXIS2_PLACEMENT_3D('',#6534,#5217,#5218);
#4636=AXIS2_PLACEMENT_3D('',#6592,#5220,#5221);
#4637=AXIS2_PLACEMENT_3D('',#6610,#5222,#5223);
#4638=AXIS2_PLACEMENT_3D('',#6612,#5225,#5226);
#4639=AXIS2_PLACEMENT_3D('',#6614,#5227,#5228);
#4640=AXIS2_PLACEMENT_3D('',#6617,#5230,#5231);
#4641=AXIS2_PLACEMENT_3D('',#6618,#5232,#5233);
#4642=AXIS2_PLACEMENT_3D('',#6619,#5234,#5235);
#4643=AXIS2_PLACEMENT_3D('',#6623,#5237,#5238);
#4644=AXIS2_PLACEMENT_3D('',#6624,#5239,#5240);
#4645=AXIS2_PLACEMENT_3D('',#6626,#5241,#5242);
#4646=AXIS2_PLACEMENT_3D('',#6684,#5244,#5245);
#4647=AXIS2_PLACEMENT_3D('',#6702,#5246,#5247);
#4648=AXIS2_PLACEMENT_3D('',#6704,#5249,#5250);
#4649=AXIS2_PLACEMENT_3D('',#6706,#5251,#5252);
#4650=AXIS2_PLACEMENT_3D('',#6709,#5254,#5255);
#4651=AXIS2_PLACEMENT_3D('',#6710,#5256,#5257);
#4652=AXIS2_PLACEMENT_3D('',#6711,#5258,#5259);
#4653=AXIS2_PLACEMENT_3D('',#6715,#5261,#5262);
#4654=AXIS2_PLACEMENT_3D('',#6716,#5263,#5264);
#4655=AXIS2_PLACEMENT_3D('',#6718,#5265,#5266);
#4656=AXIS2_PLACEMENT_3D('',#6776,#5268,#5269);
#4657=AXIS2_PLACEMENT_3D('',#6794,#5270,#5271);
#4658=AXIS2_PLACEMENT_3D('',#6796,#5273,#5274);
#4659=AXIS2_PLACEMENT_3D('',#6798,#5275,#5276);
#4660=AXIS2_PLACEMENT_3D('',#6801,#5278,#5279);
#4661=AXIS2_PLACEMENT_3D('',#6802,#5280,#5281);
#4662=AXIS2_PLACEMENT_3D('',#6803,#5282,#5283);
#4663=AXIS2_PLACEMENT_3D('',#6805,#5284,#5285);
#4664=AXIS2_PLACEMENT_3D('',#6808,#5287,#5288);
#4665=AXIS2_PLACEMENT_3D('',#6852,#5289,#5290);
#4666=AXIS2_PLACEMENT_3D('',#6854,#5291,#5292);
#4667=AXIS2_PLACEMENT_3D('',#6855,#5293,#5294);
#4668=AXIS2_PLACEMENT_3D('',#6857,#5295,#5296);
#4669=AXIS2_PLACEMENT_3D('',#6862,#5301,#5302);
#4670=AXIS2_PLACEMENT_3D('',#6864,#5303,#5304);
#4671=AXIS2_PLACEMENT_3D('',#6867,#5306,#5307);
#4672=AXIS2_PLACEMENT_3D('',#6868,#5308,#5309);
#4673=AXIS2_PLACEMENT_3D('',#6870,#5310,#5311);
#4674=AXIS2_PLACEMENT_3D('',#6871,#5312,#5313);
#4675=AXIS2_PLACEMENT_3D('',#6873,#5314,#5315);
#4676=AXIS2_PLACEMENT_3D('',#6876,#5317,#5318);
#4677=AXIS2_PLACEMENT_3D('',#6877,#5319,#5320);
#4678=AXIS2_PLACEMENT_3D('',#6879,#5321,#5322);
#4679=AXIS2_PLACEMENT_3D('',#6880,#5323,#5324);
#4680=AXIS2_PLACEMENT_3D('',#6882,#5325,#5326);
#4681=AXIS2_PLACEMENT_3D('',#6884,#5328,#5329);
#4682=AXIS2_PLACEMENT_3D('',#6886,#5330,#5331);
#4683=AXIS2_PLACEMENT_3D('',#6888,#5333,#5334);
#4684=AXIS2_PLACEMENT_3D('',#6897,#5339,#5340);
#4685=AXIS2_PLACEMENT_3D('',#6903,#5344,#5345);
#4686=AXIS2_PLACEMENT_3D('',#6909,#5349,#5350);
#4687=AXIS2_PLACEMENT_3D('',#6912,#5353,#5354);
#4688=AXIS2_PLACEMENT_3D('',#6913,#5355,#5356);
#4689=AXIS2_PLACEMENT_3D('',#6914,#5357,#5358);
#4690=AXIS2_PLACEMENT_3D('',#6915,#5359,#5360);
#4691=AXIS2_PLACEMENT_3D('',#6917,#5361,#5362);
#4692=AXIS2_PLACEMENT_3D('',#6920,#5364,#5365);
#4693=AXIS2_PLACEMENT_3D('',#6921,#5366,#5367);
#4694=AXIS2_PLACEMENT_3D('',#6922,#5368,#5369);
#4695=AXIS2_PLACEMENT_3D('',#6923,#5370,#5371);
#4696=AXIS2_PLACEMENT_3D('',#6924,#5372,#5373);
#4697=AXIS2_PLACEMENT_3D('',#6926,#5374,#5375);
#4698=AXIS2_PLACEMENT_3D('',#6929,#5377,#5378);
#4699=AXIS2_PLACEMENT_3D('',#6930,#5379,#5380);
#4700=AXIS2_PLACEMENT_3D('',#6932,#5381,#5382);
#4701=AXIS2_PLACEMENT_3D('',#6935,#5384,#5385);
#4702=AXIS2_PLACEMENT_3D('',#6936,#5386,#5387);
#4703=AXIS2_PLACEMENT_3D('',#6939,#5388,#5389);
#4704=AXIS2_PLACEMENT_3D('',#6940,#5390,#5391);
#4705=AXIS2_PLACEMENT_3D('',#6942,#5392,#5393);
#4706=AXIS2_PLACEMENT_3D('',#6945,#5395,#5396);
#4707=AXIS2_PLACEMENT_3D('',#6946,#5397,#5398);
#4708=AXIS2_PLACEMENT_3D('',#6947,#5399,#5400);
#4709=AXIS2_PLACEMENT_3D('',#6949,#5401,#5402);
#4710=AXIS2_PLACEMENT_3D('',#6952,#5404,#5405);
#4711=AXIS2_PLACEMENT_3D('',#6953,#5406,#5407);
#4712=AXIS2_PLACEMENT_3D('',#6954,#5408,#5409);
#4713=AXIS2_PLACEMENT_3D('',#6955,#5410,#5411);
#4714=AXIS2_PLACEMENT_3D('',#6956,#5412,#5413);
#4715=AXIS2_PLACEMENT_3D('',#6958,#5414,#5415);
#4716=AXIS2_PLACEMENT_3D('',#6961,#5417,#5418);
#4717=AXIS2_PLACEMENT_3D('',#6962,#5419,#5420);
#4718=AXIS2_PLACEMENT_3D('',#6964,#5421,#5422);
#4719=AXIS2_PLACEMENT_3D('',#6967,#5424,#5425);
#4720=AXIS2_PLACEMENT_3D('',#6968,#5426,#5427);
#4721=AXIS2_PLACEMENT_3D('',#6971,#5428,#5429);
#4722=AXIS2_PLACEMENT_3D('',#6972,#5430,#5431);
#4723=AXIS2_PLACEMENT_3D('',#6974,#5432,#5433);
#4724=AXIS2_PLACEMENT_3D('',#6977,#5435,#5436);
#4725=AXIS2_PLACEMENT_3D('',#6978,#5437,#5438);
#4726=AXIS2_PLACEMENT_3D('',#6979,#5439,#5440);
#4727=AXIS2_PLACEMENT_3D('',#6981,#5441,#5442);
#4728=AXIS2_PLACEMENT_3D('',#6984,#5444,#5445);
#4729=AXIS2_PLACEMENT_3D('',#6985,#5446,#5447);
#4730=AXIS2_PLACEMENT_3D('',#6986,#5448,#5449);
#4731=AXIS2_PLACEMENT_3D('',#6987,#5450,#5451);
#4732=AXIS2_PLACEMENT_3D('',#6988,#5452,#5453);
#4733=AXIS2_PLACEMENT_3D('',#6990,#5454,#5455);
#4734=AXIS2_PLACEMENT_3D('',#6993,#5457,#5458);
#4735=AXIS2_PLACEMENT_3D('',#6994,#5459,#5460);
#4736=AXIS2_PLACEMENT_3D('',#6996,#5461,#5462);
#4737=AXIS2_PLACEMENT_3D('',#6999,#5464,#5465);
#4738=AXIS2_PLACEMENT_3D('',#7000,#5466,#5467);
#4739=AXIS2_PLACEMENT_3D('',#7003,#5468,#5469);
#4740=AXIS2_PLACEMENT_3D('',#7004,#5470,#5471);
#4741=AXIS2_PLACEMENT_3D('',#7006,#5472,#5473);
#4742=AXIS2_PLACEMENT_3D('',#7009,#5475,#5476);
#4743=AXIS2_PLACEMENT_3D('',#7010,#5477,#5478);
#4744=AXIS2_PLACEMENT_3D('',#7011,#5479,#5480);
#4745=AXIS2_PLACEMENT_3D('',#7013,#5481,#5482);
#4746=AXIS2_PLACEMENT_3D('',#7016,#5484,#5485);
#4747=AXIS2_PLACEMENT_3D('',#7017,#5486,#5487);
#4748=AXIS2_PLACEMENT_3D('',#7018,#5488,#5489);
#4749=AXIS2_PLACEMENT_3D('',#7019,#5490,#5491);
#4750=AXIS2_PLACEMENT_3D('',#7020,#5492,#5493);
#4751=AXIS2_PLACEMENT_3D('',#7029,#5498,#5499);
#4752=AXIS2_PLACEMENT_3D('',#7035,#5503,#5504);
#4753=AXIS2_PLACEMENT_3D('',#7041,#5508,#5509);
#4754=AXIS2_PLACEMENT_3D('',#7047,#5513,#5514);
#4755=AXIS2_PLACEMENT_3D('',#7053,#5518,#5519);
#4756=AXIS2_PLACEMENT_3D('',#7059,#5523,#5524);
#4757=AXIS2_PLACEMENT_3D('',#7065,#5528,#5529);
#4758=AXIS2_PLACEMENT_3D('',#7071,#5533,#5534);
#4759=AXIS2_PLACEMENT_3D('',#7077,#5538,#5539);
#4760=AXIS2_PLACEMENT_3D('',#7086,#5544,#5545);
#4761=AXIS2_PLACEMENT_3D('',#7092,#5549,#5550);
#4762=AXIS2_PLACEMENT_3D('',#7098,#5554,#5555);
#4763=AXIS2_PLACEMENT_3D('',#7104,#5559,#5560);
#4764=AXIS2_PLACEMENT_3D('',#7110,#5564,#5565);
#4765=AXIS2_PLACEMENT_3D('',#7116,#5569,#5570);
#4766=AXIS2_PLACEMENT_3D('',#7122,#5574,#5575);
#4767=AXIS2_PLACEMENT_3D('',#7128,#5579,#5580);
#4768=AXIS2_PLACEMENT_3D('',#7134,#5584,#5585);
#4769=AXIS2_PLACEMENT_3D('',#7143,#5590,#5591);
#4770=AXIS2_PLACEMENT_3D('',#7149,#5595,#5596);
#4771=AXIS2_PLACEMENT_3D('',#7155,#5600,#5601);
#4772=AXIS2_PLACEMENT_3D('',#7161,#5605,#5606);
#4773=AXIS2_PLACEMENT_3D('',#7167,#5610,#5611);
#4774=AXIS2_PLACEMENT_3D('',#7173,#5615,#5616);
#4775=AXIS2_PLACEMENT_3D('',#7179,#5620,#5621);
#4776=AXIS2_PLACEMENT_3D('',#7185,#5625,#5626);
#4777=AXIS2_PLACEMENT_3D('',#7191,#5630,#5631);
#4778=AXIS2_PLACEMENT_3D('',#7200,#5636,#5637);
#4779=AXIS2_PLACEMENT_3D('',#7206,#5641,#5642);
#4780=AXIS2_PLACEMENT_3D('',#7212,#5646,#5647);
#4781=AXIS2_PLACEMENT_3D('',#7218,#5651,#5652);
#4782=AXIS2_PLACEMENT_3D('',#7224,#5656,#5657);
#4783=AXIS2_PLACEMENT_3D('',#7230,#5661,#5662);
#4784=AXIS2_PLACEMENT_3D('',#7236,#5666,#5667);
#4785=AXIS2_PLACEMENT_3D('',#7242,#5671,#5672);
#4786=AXIS2_PLACEMENT_3D('',#7248,#5676,#5677);
#4787=AXIS2_PLACEMENT_3D('',#7250,#5678,#5679);
#4788=AXIS2_PLACEMENT_3D('',#7253,#5681,#5682);
#4789=AXIS2_PLACEMENT_3D('',#7254,#5683,#5684);
#4790=AXIS2_PLACEMENT_3D('',#7260,#5688,#5689);
#4791=AXIS2_PLACEMENT_3D('',#7266,#5693,#5694);
#4792=AXIS2_PLACEMENT_3D('',#7269,#5697,#5698);
#4793=AXIS2_PLACEMENT_3D('',#7275,#5702,#5703);
#4794=AXIS2_PLACEMENT_3D('',#7278,#5706,#5707);
#4795=AXIS2_PLACEMENT_3D('',#7284,#5711,#5712);
#4796=AXIS2_PLACEMENT_3D('',#7287,#5715,#5716);
#4797=AXIS2_PLACEMENT_3D('',#7290,#5719,#5720);
#4798=AXIS2_PLACEMENT_3D('',#7291,#5721,#5722);
#4799=AXIS2_PLACEMENT_3D('',#7292,#5723,#5724);
#4800=AXIS2_PLACEMENT_3D('',#7293,#5725,#5726);
#4801=AXIS2_PLACEMENT_3D('',#7295,#5727,#5728);
#4802=AXIS2_PLACEMENT_3D('',#7298,#5730,#5731);
#4803=AXIS2_PLACEMENT_3D('',#7299,#5732,#5733);
#4804=AXIS2_PLACEMENT_3D('',#7302,#5735,#5736);
#4805=AXIS2_PLACEMENT_3D('',#7303,#5737,#5738);
#4806=AXIS2_PLACEMENT_3D('',#7305,#5739,#5740);
#4807=AXIS2_PLACEMENT_3D('',#7306,#5741,#5742);
#4808=AXIS2_PLACEMENT_3D('',#7309,#5744,#5745);
#4809=AXIS2_PLACEMENT_3D('',#7310,#5746,#5747);
#4810=AXIS2_PLACEMENT_3D('',#7311,#5748,#5749);
#4811=AXIS2_PLACEMENT_3D('',#7312,#5750,#5751);
#4812=AXIS2_PLACEMENT_3D('',#7321,#5756,#5757);
#4813=AXIS2_PLACEMENT_3D('',#7327,#5761,#5762);
#4814=AXIS2_PLACEMENT_3D('',#7333,#5766,#5767);
#4815=AXIS2_PLACEMENT_3D('',#7339,#5771,#5772);
#4816=AXIS2_PLACEMENT_3D('',#7345,#5776,#5777);
#4817=AXIS2_PLACEMENT_3D('',#7348,#5780,#5781);
#4818=AXIS2_PLACEMENT_3D('',#7349,#5782,#5783);
#4819=AXIS2_PLACEMENT_3D('',#7350,#5784,#5785);
#4820=AXIS2_PLACEMENT_3D('',#7352,#5786,#5787);
#4821=AXIS2_PLACEMENT_3D('',#7353,#5788,#5789);
#4822=AXIS2_PLACEMENT_3D('',#7355,#5790,#5791);
#4823=AXIS2_PLACEMENT_3D('',#7356,#5792,#5793);
#4824=AXIS2_PLACEMENT_3D('',#7358,#5794,#5795);
#4825=AXIS2_PLACEMENT_3D('',#7360,#5797,#5798);
#4826=AXIS2_PLACEMENT_3D('',#7362,#5799,#5800);
#4827=AXIS2_PLACEMENT_3D('',#7364,#5802,#5803);
#4828=AXIS2_PLACEMENT_3D('',#7366,#5804,#5805);
#4829=AXIS2_PLACEMENT_3D('',#7368,#5807,#5808);
#4830=AXIS2_PLACEMENT_3D('',#7370,#5809,#5810);
#4831=AXIS2_PLACEMENT_3D('',#7371,#5811,#5812);
#4832=AXIS2_PLACEMENT_3D('',#7373,#5813,#5814);
#4833=AXIS2_PLACEMENT_3D('',#7375,#5816,#5817);
#4834=AXIS2_PLACEMENT_3D('',#7377,#5819,#5820);
#4835=AXIS2_PLACEMENT_3D('',#7378,#5821,#5822);
#4836=AXIS2_PLACEMENT_3D('',#7380,#5823,#5824);
#4837=AXIS2_PLACEMENT_3D('',#7381,#5825,#5826);
#4838=AXIS2_PLACEMENT_3D('',#7383,#5827,#5828);
#4839=AXIS2_PLACEMENT_3D('',#7385,#5830,#5831);
#4840=AXIS2_PLACEMENT_3D('',#7387,#5832,#5833);
#4841=AXIS2_PLACEMENT_3D('',#7389,#5835,#5836);
#4842=AXIS2_PLACEMENT_3D('',#7391,#5837,#5838);
#4843=AXIS2_PLACEMENT_3D('',#7393,#5840,#5841);
#4844=AXIS2_PLACEMENT_3D('',#7395,#5842,#5843);
#4845=AXIS2_PLACEMENT_3D('',#7396,#5844,#5845);
#4846=AXIS2_PLACEMENT_3D('',#7398,#5846,#5847);
#4847=AXIS2_PLACEMENT_3D('',#7400,#5849,#5850);
#4848=AXIS2_PLACEMENT_3D('',#7402,#5851,#5852);
#4849=AXIS2_PLACEMENT_3D('',#7404,#5854,#5855);
#4850=AXIS2_PLACEMENT_3D('',#7406,#5856,#5857);
#4851=AXIS2_PLACEMENT_3D('',#7408,#5859,#5860);
#4852=AXIS2_PLACEMENT_3D('',#7409,#5861,#5862);
#4853=AXIS2_PLACEMENT_3D('',#7418,#5867,#5868);
#4854=AXIS2_PLACEMENT_3D('',#7424,#5872,#5873);
#4855=AXIS2_PLACEMENT_3D('',#7430,#5877,#5878);
#4856=AXIS2_PLACEMENT_3D('',#7436,#5882,#5883);
#4857=AXIS2_PLACEMENT_3D('',#7442,#5887,#5888);
#4858=AXIS2_PLACEMENT_3D('',#7445,#5891,#5892);
#4859=AXIS2_PLACEMENT_3D('',#7446,#5893,#5894);
#4860=AXIS2_PLACEMENT_3D('',#7447,#5895,#5896);
#4861=AXIS2_PLACEMENT_3D('',#7448,#5897,#5898);
#4862=AXIS2_PLACEMENT_3D('',#7462,#5905,#5906);
#4863=AXIS2_PLACEMENT_3D('',#7463,#5907,#5908);
#4864=AXIS2_PLACEMENT_3D('',#7477,#5915,#5916);
#4865=AXIS2_PLACEMENT_3D('',#7478,#5917,#5918);
#4866=AXIS2_PLACEMENT_3D('',#7481,#5921,#5922);
#4867=AXIS2_PLACEMENT_3D('',#7483,#5924,#5925);
#4868=AXIS2_PLACEMENT_3D('',#7485,#5927,#5928);
#4869=AXIS2_PLACEMENT_3D('',#7487,#5930,#5931);
#4870=AXIS2_PLACEMENT_3D('',#7489,#5933,#5934);
#4871=AXIS2_PLACEMENT_3D('',#7490,#5935,#5936);
#4872=AXIS2_PLACEMENT_3D('',#7493,#5938,#5939);
#4873=AXIS2_PLACEMENT_3D('',#7494,#5940,#5941);
#4874=AXIS2_PLACEMENT_3D('',#7496,#5942,#5943);
#4875=AXIS2_PLACEMENT_3D('',#7498,#5944,#5945);
#4876=AXIS2_PLACEMENT_3D('',#7499,#5946,#5947);
#4877=AXIS2_PLACEMENT_3D('',#7501,#5949,#5950);
#4878=AXIS2_PLACEMENT_3D('',#7503,#5951,#5952);
#4879=AXIS2_PLACEMENT_3D('',#7505,#5954,#5955);
#4880=AXIS2_PLACEMENT_3D('',#7507,#5956,#5957);
#4881=AXIS2_PLACEMENT_3D('',#7509,#5959,#5960);
#4882=AXIS2_PLACEMENT_3D('',#7511,#5961,#5962);
#4883=AXIS2_PLACEMENT_3D('',#7512,#5963,#5964);
#4884=AXIS2_PLACEMENT_3D('',#7514,#5966,#5967);
#4885=AXIS2_PLACEMENT_3D('',#7515,#5968,#5969);
#4886=AXIS2_PLACEMENT_3D('',#7516,#5970,#5971);
#4887=AXIS2_PLACEMENT_3D('',#7517,#5972,#5973);
#4888=AXIS2_PLACEMENT_3D('',#7518,#5974,#5975);
#4889=AXIS2_PLACEMENT_3D('',#7519,#5976,#5977);
#4890=AXIS2_PLACEMENT_3D('',#7520,#5978,#5979);
#4891=AXIS2_PLACEMENT_3D('',#7521,#5980,#5981);
#4892=AXIS2_PLACEMENT_3D('',#7522,#5982,#5983);
#4893=AXIS2_PLACEMENT_3D('',#7523,#5984,#5985);
#4894=AXIS2_PLACEMENT_3D('',#7524,#5986,#5987);
#4895=AXIS2_PLACEMENT_3D('',#7525,#5988,#5989);
#4896=AXIS2_PLACEMENT_3D('',#7526,#5990,#5991);
#4897=AXIS2_PLACEMENT_3D('',#7527,#5992,#5993);
#4898=AXIS2_PLACEMENT_3D('',#7528,#5994,#5995);
#4899=AXIS2_PLACEMENT_3D('',#7529,#5996,#5997);
#4900=AXIS2_PLACEMENT_3D('',#7530,#5998,#5999);
#4901=AXIS2_PLACEMENT_3D('',#7531,#6000,#6001);
#4902=AXIS2_PLACEMENT_3D('',#7532,#6002,#6003);
#4903=AXIS2_PLACEMENT_3D('',#7533,#6004,#6005);
#4904=AXIS2_PLACEMENT_3D('',#7535,#6006,#6007);
#4905=AXIS2_PLACEMENT_3D('',#7538,#6009,#6010);
#4906=AXIS2_PLACEMENT_3D('',#7539,#6011,#6012);
#4907=AXIS2_PLACEMENT_3D('',#7541,#6013,#6014);
#4908=AXIS2_PLACEMENT_3D('',#7542,#6015,#6016);
#4909=AXIS2_PLACEMENT_3D('',#7545,#6018,#6019);
#4910=AXIS2_PLACEMENT_3D('',#7546,#6020,#6021);
#4911=AXIS2_PLACEMENT_3D('',#7548,#6022,#6023);
#4912=AXIS2_PLACEMENT_3D('',#7551,#6025,#6026);
#4913=AXIS2_PLACEMENT_3D('',#7552,#6027,#6028);
#4914=AXIS2_PLACEMENT_3D('',#7553,#6029,#6030);
#4915=AXIS2_PLACEMENT_3D('',#7556,#6031,#6032);
#4916=AXIS2_PLACEMENT_3D('',#7557,#6033,#6034);
#4917=AXIS2_PLACEMENT_3D('',#7558,#6035,#6036);
#4918=AXIS2_PLACEMENT_3D('',#7560,#6037,#6038);
#4919=AXIS2_PLACEMENT_3D('',#7563,#6040,#6041);
#4920=AXIS2_PLACEMENT_3D('',#7564,#6042,#6043);
#4921=AXIS2_PLACEMENT_3D('',#7566,#6044,#6045);
#4922=AXIS2_PLACEMENT_3D('',#7569,#6047,#6048);
#4923=AXIS2_PLACEMENT_3D('',#7570,#6049,#6050);
#4924=AXIS2_PLACEMENT_3D('',#7571,#6051,#6052);
#4925=AXIS2_PLACEMENT_3D('',#7572,#6053,#6054);
#4926=AXIS2_PLACEMENT_3D('',#7573,#6055,#6056);
#4927=AXIS2_PLACEMENT_3D('',#7575,#6057,#6058);
#4928=AXIS2_PLACEMENT_3D('',#7578,#6060,#6061);
#4929=AXIS2_PLACEMENT_3D('',#7579,#6062,#6063);
#4930=AXIS2_PLACEMENT_3D('',#7581,#6064,#6065);
#4931=AXIS2_PLACEMENT_3D('',#7582,#6066,#6067);
#4932=AXIS2_PLACEMENT_3D('',#7585,#6069,#6070);
#4933=AXIS2_PLACEMENT_3D('',#7586,#6071,#6072);
#4934=AXIS2_PLACEMENT_3D('',#7588,#6073,#6074);
#4935=AXIS2_PLACEMENT_3D('',#7591,#6076,#6077);
#4936=AXIS2_PLACEMENT_3D('',#7592,#6078,#6079);
#4937=AXIS2_PLACEMENT_3D('',#7593,#6080,#6081);
#4938=AXIS2_PLACEMENT_3D('',#7594,#6082,#6083);
#4939=AXIS2_PLACEMENT_3D('',#7595,#6084,#6085);
#4940=AXIS2_PLACEMENT_3D('',#7596,#6086,#6087);
#4941=AXIS2_PLACEMENT_3D('',#7598,#6088,#6089);
#4942=AXIS2_PLACEMENT_3D('',#7601,#6091,#6092);
#4943=AXIS2_PLACEMENT_3D('',#7602,#6093,#6094);
#4944=AXIS2_PLACEMENT_3D('',#7604,#6095,#6096);
#4945=AXIS2_PLACEMENT_3D('',#7605,#6097,#6098);
#4946=AXIS2_PLACEMENT_3D('',#7608,#6100,#6101);
#4947=AXIS2_PLACEMENT_3D('',#7609,#6102,#6103);
#4948=AXIS2_PLACEMENT_3D('',#7611,#6104,#6105);
#4949=AXIS2_PLACEMENT_3D('',#7614,#6107,#6108);
#4950=AXIS2_PLACEMENT_3D('',#7615,#6109,#6110);
#4951=AXIS2_PLACEMENT_3D('',#7616,#6111,#6112);
#4952=AXIS2_PLACEMENT_3D('',#7619,#6113,#6114);
#4953=AXIS2_PLACEMENT_3D('',#7620,#6115,#6116);
#4954=AXIS2_PLACEMENT_3D('',#7621,#6117,#6118);
#4955=AXIS2_PLACEMENT_3D('',#7623,#6119,#6120);
#4956=AXIS2_PLACEMENT_3D('',#7626,#6122,#6123);
#4957=AXIS2_PLACEMENT_3D('',#7627,#6124,#6125);
#4958=AXIS2_PLACEMENT_3D('',#7629,#6126,#6127);
#4959=AXIS2_PLACEMENT_3D('',#7632,#6129,#6130);
#4960=AXIS2_PLACEMENT_3D('',#7633,#6131,#6132);
#4961=AXIS2_PLACEMENT_3D('',#7634,#6133,#6134);
#4962=AXIS2_PLACEMENT_3D('',#7635,#6135,#6136);
#4963=AXIS2_PLACEMENT_3D('',#7636,#6137,#6138);
#4964=AXIS2_PLACEMENT_3D('',#7638,#6139,#6140);
#4965=AXIS2_PLACEMENT_3D('',#7641,#6142,#6143);
#4966=AXIS2_PLACEMENT_3D('',#7642,#6144,#6145);
#4967=AXIS2_PLACEMENT_3D('',#7644,#6146,#6147);
#4968=AXIS2_PLACEMENT_3D('',#7645,#6148,#6149);
#4969=AXIS2_PLACEMENT_3D('',#7648,#6151,#6152);
#4970=AXIS2_PLACEMENT_3D('',#7649,#6153,#6154);
#4971=AXIS2_PLACEMENT_3D('',#7651,#6155,#6156);
#4972=AXIS2_PLACEMENT_3D('',#7654,#6158,#6159);
#4973=AXIS2_PLACEMENT_3D('',#7655,#6160,#6161);
#4974=AXIS2_PLACEMENT_3D('',#7656,#6162,#6163);
#4975=AXIS2_PLACEMENT_3D('',#7657,#6164,#6165);
#4976=AXIS2_PLACEMENT_3D('',#7658,#6166,#6167);
#4977=AXIS2_PLACEMENT_3D('',#7659,#6168,#6169);
#4978=AXIS2_PLACEMENT_3D('',#7661,#6170,#6171);
#4979=AXIS2_PLACEMENT_3D('',#7664,#6173,#6174);
#4980=AXIS2_PLACEMENT_3D('',#7665,#6175,#6176);
#4981=AXIS2_PLACEMENT_3D('',#7667,#6177,#6178);
#4982=AXIS2_PLACEMENT_3D('',#7668,#6179,#6180);
#4983=AXIS2_PLACEMENT_3D('',#7671,#6182,#6183);
#4984=AXIS2_PLACEMENT_3D('',#7672,#6184,#6185);
#4985=AXIS2_PLACEMENT_3D('',#7674,#6186,#6187);
#4986=AXIS2_PLACEMENT_3D('',#7677,#6189,#6190);
#4987=AXIS2_PLACEMENT_3D('',#7678,#6191,#6192);
#4988=AXIS2_PLACEMENT_3D('',#7679,#6193,#6194);
#4989=AXIS2_PLACEMENT_3D('',#7682,#6195,#6196);
#4990=AXIS2_PLACEMENT_3D('',#7683,#6197,#6198);
#4991=AXIS2_PLACEMENT_3D('',#7684,#6199,#6200);
#4992=AXIS2_PLACEMENT_3D('',#7686,#6201,#6202);
#4993=AXIS2_PLACEMENT_3D('',#7689,#6204,#6205);
#4994=AXIS2_PLACEMENT_3D('',#7690,#6206,#6207);
#4995=AXIS2_PLACEMENT_3D('',#7692,#6208,#6209);
#4996=AXIS2_PLACEMENT_3D('',#7695,#6211,#6212);
#4997=AXIS2_PLACEMENT_3D('',#7696,#6213,#6214);
#4998=AXIS2_PLACEMENT_3D('',#7697,#6215,#6216);
#4999=AXIS2_PLACEMENT_3D('',#7698,#6217,#6218);
#5000=AXIS2_PLACEMENT_3D('',#7699,#6219,#6220);
#5001=AXIS2_PLACEMENT_3D('',#7701,#6221,#6222);
#5002=AXIS2_PLACEMENT_3D('',#7704,#6224,#6225);
#5003=AXIS2_PLACEMENT_3D('',#7705,#6226,#6227);
#5004=AXIS2_PLACEMENT_3D('',#7707,#6228,#6229);
#5005=AXIS2_PLACEMENT_3D('',#7708,#6230,#6231);
#5006=AXIS2_PLACEMENT_3D('',#7711,#6233,#6234);
#5007=AXIS2_PLACEMENT_3D('',#7712,#6235,#6236);
#5008=AXIS2_PLACEMENT_3D('',#7714,#6237,#6238);
#5009=AXIS2_PLACEMENT_3D('',#7717,#6240,#6241);
#5010=AXIS2_PLACEMENT_3D('',#7718,#6242,#6243);
#5011=AXIS2_PLACEMENT_3D('',#7719,#6244,#6245);
#5012=AXIS2_PLACEMENT_3D('',#7720,#6246,#6247);
#5013=AXIS2_PLACEMENT_3D('',#7721,#6248,#6249);
#5014=AXIS2_PLACEMENT_3D('',#7722,#6250,#6251);
#5015=AXIS2_PLACEMENT_3D('',#7724,#6252,#6253);
#5016=AXIS2_PLACEMENT_3D('',#7727,#6255,#6256);
#5017=AXIS2_PLACEMENT_3D('',#7728,#6257,#6258);
#5018=AXIS2_PLACEMENT_3D('',#7730,#6259,#6260);
#5019=AXIS2_PLACEMENT_3D('',#7731,#6261,#6262);
#5020=AXIS2_PLACEMENT_3D('',#7745,#6269,#6270);
#5021=AXIS2_PLACEMENT_3D('',#7746,#6271,#6272);
#5022=AXIS2_PLACEMENT_3D('',#7760,#6279,#6280);
#5023=AXIS2_PLACEMENT_3D('',#7761,#6281,#6282);
#5024=AXIS2_PLACEMENT_3D('',#7764,#6285,#6286);
#5025=AXIS2_PLACEMENT_3D('',#7766,#6288,#6289);
#5026=AXIS2_PLACEMENT_3D('',#7768,#6291,#6292);
#5027=AXIS2_PLACEMENT_3D('',#7770,#6294,#6295);
#5028=AXIS2_PLACEMENT_3D('',#7772,#6297,#6298);
#5029=AXIS2_PLACEMENT_3D('',#7773,#6299,#6300);
#5030=AXIS2_PLACEMENT_3D('',#7775,#6301,#6302);
#5031=AXIS2_PLACEMENT_3D('',#7776,#6303,#6304);
#5032=AXIS2_PLACEMENT_3D('',#7779,#6306,#6307);
#5033=AXIS2_PLACEMENT_3D('',#7780,#6308,#6309);
#5034=AXIS2_PLACEMENT_3D('',#7782,#6310,#6311);
#5035=AXIS2_PLACEMENT_3D('',#7783,#6312,#6313);
#5036=AXIS2_PLACEMENT_3D('',#7785,#6315,#6316);
#5037=AXIS2_PLACEMENT_3D('',#7787,#6317,#6318);
#5038=AXIS2_PLACEMENT_3D('',#7789,#6320,#6321);
#5039=AXIS2_PLACEMENT_3D('',#7791,#6322,#6323);
#5040=AXIS2_PLACEMENT_3D('',#7792,#6324,#6325);
#5041=AXIS2_PLACEMENT_3D('',#7794,#6327,#6328);
#5042=AXIS2_PLACEMENT_3D('',#7795,#6329,#6330);
#5043=AXIS2_PLACEMENT_3D('',#7797,#6331,#6332);
#5044=AXIS2_PLACEMENT_3D('',#7799,#6333,#6334);
#5045=AXIS2_PLACEMENT_3D('',#7800,#6335,#6336);
#5046=AXIS2_PLACEMENT_3D('',#7802,#6337,#6338);
#5047=AXIS2_PLACEMENT_3D('',#7804,#6340,#6341);
#5048=AXIS2_PLACEMENT_3D('',#7806,#6342,#6343);
#5049=AXIS2_PLACEMENT_3D('',#7807,#6344,#6345);
#5050=AXIS2_PLACEMENT_3D('',#7809,#6346,#6347);
#5051=AXIS2_PLACEMENT_3D('',#7811,#6349,#6350);
#5052=AXIS2_PLACEMENT_3D('',#7813,#6351,#6352);
#5053=AXIS2_PLACEMENT_3D('',#7814,#6353,#6354);
#5054=AXIS2_PLACEMENT_3D('',#7816,#6356,#6357);
#5055=AXIS2_PLACEMENT_3D('',#7817,#6358,#6359);
#5056=AXIS2_PLACEMENT_3D('',#7818,#6360,#6361);
#5057=AXIS2_PLACEMENT_3D('',#7819,#6362,#6363);
#5058=AXIS2_PLACEMENT_3D('',#7820,#6364,#6365);
#5059=AXIS2_PLACEMENT_3D('',#7821,#6366,#6367);
#5060=AXIS2_PLACEMENT_3D('',#7822,#6368,#6369);
#5061=AXIS2_PLACEMENT_3D('',#7823,#6370,#6371);
#5062=AXIS2_PLACEMENT_3D('',#7824,#6372,#6373);
#5063=AXIS2_PLACEMENT_3D('',#7825,#6374,#6375);
#5064=AXIS2_PLACEMENT_3D('',#7826,#6376,#6377);
#5065=AXIS2_PLACEMENT_3D('',#7827,#6378,#6379);
#5066=AXIS2_PLACEMENT_3D('',#7828,#6380,#6381);
#5067=AXIS2_PLACEMENT_3D('',#7829,#6382,#6383);
#5068=AXIS2_PLACEMENT_3D('',#7830,#6384,#6385);
#5069=AXIS2_PLACEMENT_3D('',#7831,#6386,#6387);
#5070=AXIS2_PLACEMENT_3D('',#7832,#6388,#6389);
#5071=AXIS2_PLACEMENT_3D('',#7833,#6390,#6391);
#5072=DIRECTION('axis',(0.,0.,1.));
#5073=DIRECTION('refdir',(1.,0.,0.));
#5074=DIRECTION('axis',(0.,0.,1.));
#5075=DIRECTION('refdir',(1.,0.,0.));
#5076=DIRECTION('axis',(0.,0.,1.));
#5077=DIRECTION('refdir',(1.,0.,0.));
#5078=DIRECTION('center_axis',(0.,0.,1.));
#5079=DIRECTION('ref_axis',(1.,0.,0.));
#5080=DIRECTION('center_axis',(0.,0.,1.));
#5081=DIRECTION('ref_axis',(1.,0.,0.));
#5082=DIRECTION('',(0.,0.,1.));
#5083=DIRECTION('center_axis',(0.,0.,-1.));
#5084=DIRECTION('ref_axis',(1.,0.,0.));
#5085=DIRECTION('center_axis',(0.,1.,0.));
#5086=DIRECTION('ref_axis',(-1.,0.,0.));
#5087=DIRECTION('',(-1.,0.,0.));
#5088=DIRECTION('',(0.,0.,1.));
#5089=DIRECTION('',(-1.,0.,0.));
#5090=DIRECTION('',(0.,0.,1.));
#5091=DIRECTION('center_axis',(1.,0.,0.));
#5092=DIRECTION('ref_axis',(0.,1.,0.));
#5093=DIRECTION('',(0.,1.,0.));
#5094=DIRECTION('',(0.,1.,0.));
#5095=DIRECTION('',(0.,0.,1.));
#5096=DIRECTION('center_axis',(0.,-1.,0.));
#5097=DIRECTION('ref_axis',(1.,0.,0.));
#5098=DIRECTION('',(1.,0.,0.));
#5099=DIRECTION('',(1.,0.,0.));
#5100=DIRECTION('',(0.,0.,1.));
#5101=DIRECTION('center_axis',(-1.,0.,0.));
#5102=DIRECTION('ref_axis',(0.,-1.,0.));
#5103=DIRECTION('',(0.,-1.,0.));
#5104=DIRECTION('',(0.,-1.,0.));
#5105=DIRECTION('center_axis',(0.,0.,1.));
#5106=DIRECTION('ref_axis',(1.,0.,0.));
#5107=DIRECTION('center_axis',(0.,0.,1.));
#5108=DIRECTION('ref_axis',(1.,0.,0.));
#5109=DIRECTION('axis',(0.,0.,1.));
#5110=DIRECTION('refdir',(1.,0.,0.));
#5111=DIRECTION('center_axis',(0.,1.,0.));
#5112=DIRECTION('ref_axis',(-1.,0.,0.));
#5113=DIRECTION('',(-1.,0.,0.));
#5114=DIRECTION('',(0.,0.,1.));
#5115=DIRECTION('',(-1.,0.,0.));
#5116=DIRECTION('',(0.,0.,1.));
#5117=DIRECTION('center_axis',(1.,0.,0.));
#5118=DIRECTION('ref_axis',(0.,1.,0.));
#5119=DIRECTION('',(0.,1.,0.));
#5120=DIRECTION('',(0.,1.,0.));
#5121=DIRECTION('',(0.,0.,1.));
#5122=DIRECTION('center_axis',(0.,-1.,0.));
#5123=DIRECTION('ref_axis',(1.,0.,0.));
#5124=DIRECTION('',(1.,0.,0.));
#5125=DIRECTION('',(1.,0.,0.));
#5126=DIRECTION('',(0.,0.,1.));
#5127=DIRECTION('center_axis',(-1.,0.,0.));
#5128=DIRECTION('ref_axis',(0.,-1.,0.));
#5129=DIRECTION('',(0.,-1.,0.));
#5130=DIRECTION('',(0.,-1.,0.));
#5131=DIRECTION('center_axis',(0.,0.,1.));
#5132=DIRECTION('ref_axis',(1.,0.,0.));
#5133=DIRECTION('center_axis',(0.,0.,1.));
#5134=DIRECTION('ref_axis',(1.,0.,0.));
#5135=DIRECTION('axis',(0.,0.,1.));
#5136=DIRECTION('refdir',(1.,0.,0.));
#5137=DIRECTION('center_axis',(0.,1.,0.));
#5138=DIRECTION('ref_axis',(-1.,0.,0.));
#5139=DIRECTION('',(-1.,0.,0.));
#5140=DIRECTION('',(0.,0.,1.));
#5141=DIRECTION('',(-1.,0.,0.));
#5142=DIRECTION('',(0.,0.,1.));
#5143=DIRECTION('center_axis',(1.,0.,0.));
#5144=DIRECTION('ref_axis',(0.,1.,0.));
#5145=DIRECTION('',(0.,1.,0.));
#5146=DIRECTION('',(0.,1.,0.));
#5147=DIRECTION('',(0.,0.,1.));
#5148=DIRECTION('center_axis',(0.,-1.,0.));
#5149=DIRECTION('ref_axis',(1.,0.,0.));
#5150=DIRECTION('',(1.,0.,0.));
#5151=DIRECTION('',(1.,0.,0.));
#5152=DIRECTION('',(0.,0.,1.));
#5153=DIRECTION('center_axis',(-1.,0.,0.));
#5154=DIRECTION('ref_axis',(0.,-1.,0.));
#5155=DIRECTION('',(0.,-1.,0.));
#5156=DIRECTION('',(0.,-1.,0.));
#5157=DIRECTION('center_axis',(0.,0.,1.));
#5158=DIRECTION('ref_axis',(1.,0.,0.));
#5159=DIRECTION('center_axis',(0.,0.,1.));
#5160=DIRECTION('ref_axis',(1.,0.,0.));
#5161=DIRECTION('axis',(0.,0.,1.));
#5162=DIRECTION('refdir',(1.,0.,0.));
#5163=DIRECTION('center_axis',(0.,0.,1.));
#5164=DIRECTION('ref_axis',(1.,0.,0.));
#5165=DIRECTION('center_axis',(0.,0.,1.));
#5166=DIRECTION('ref_axis',(1.,0.,0.));
#5167=DIRECTION('',(0.,0.,1.));
#5168=DIRECTION('center_axis',(0.,0.,-1.));
#5169=DIRECTION('ref_axis',(1.,0.,0.));
#5170=DIRECTION('center_axis',(0.,0.,1.));
#5171=DIRECTION('ref_axis',(1.,0.,0.));
#5172=DIRECTION('center_axis',(0.,0.,1.));
#5173=DIRECTION('ref_axis',(1.,0.,0.));
#5174=DIRECTION('',(0.,0.,1.));
#5175=DIRECTION('center_axis',(0.,0.,-1.));
#5176=DIRECTION('ref_axis',(1.,0.,0.));
#5177=DIRECTION('center_axis',(0.,0.,1.));
#5178=DIRECTION('ref_axis',(1.,0.,0.));
#5179=DIRECTION('center_axis',(0.,0.,1.));
#5180=DIRECTION('ref_axis',(1.,0.,0.));
#5181=DIRECTION('',(0.,0.,1.));
#5182=DIRECTION('center_axis',(0.,0.,-1.));
#5183=DIRECTION('ref_axis',(1.,0.,0.));
#5184=DIRECTION('center_axis',(0.,1.,0.));
#5185=DIRECTION('ref_axis',(-1.,0.,0.));
#5186=DIRECTION('',(-1.,0.,0.));
#5187=DIRECTION('',(0.,0.,1.));
#5188=DIRECTION('',(-1.,0.,0.));
#5189=DIRECTION('',(0.,0.,1.));
#5190=DIRECTION('center_axis',(1.,0.,0.));
#5191=DIRECTION('ref_axis',(0.,1.,0.));
#5192=DIRECTION('',(0.,1.,0.));
#5193=DIRECTION('',(0.,1.,0.));
#5194=DIRECTION('',(0.,0.,1.));
#5195=DIRECTION('center_axis',(0.,-1.,0.));
#5196=DIRECTION('ref_axis',(1.,0.,0.));
#5197=DIRECTION('',(1.,0.,0.));
#5198=DIRECTION('',(1.,0.,0.));
#5199=DIRECTION('',(0.,0.,1.));
#5200=DIRECTION('center_axis',(-1.,0.,0.));
#5201=DIRECTION('ref_axis',(0.,-1.,0.));
#5202=DIRECTION('',(0.,-1.,0.));
#5203=DIRECTION('',(0.,-1.,0.));
#5204=DIRECTION('center_axis',(0.,0.,1.));
#5205=DIRECTION('ref_axis',(1.,0.,0.));
#5206=DIRECTION('center_axis',(0.,0.,1.));
#5207=DIRECTION('ref_axis',(1.,0.,0.));
#5208=DIRECTION('axis',(0.,0.,1.));
#5209=DIRECTION('refdir',(1.,0.,0.));
#5210=DIRECTION('center_axis',(0.,1.,0.));
#5211=DIRECTION('ref_axis',(1.,0.,0.));
#5212=DIRECTION('',(-1.,0.,0.));
#5213=DIRECTION('center_axis',(0.,1.,0.));
#5214=DIRECTION('ref_axis',(1.,0.,0.));
#5215=DIRECTION('center_axis',(0.,1.,0.));
#5216=DIRECTION('ref_axis',(1.,0.,0.));
#5217=DIRECTION('center_axis',(0.,1.,0.));
#5218=DIRECTION('ref_axis',(1.,0.,0.));
#5219=DIRECTION('',(0.,1.,0.));
#5220=DIRECTION('center_axis',(0.,1.,0.));
#5221=DIRECTION('ref_axis',(1.,0.,0.));
#5222=DIRECTION('center_axis',(0.,1.,0.));
#5223=DIRECTION('ref_axis',(1.,0.,0.));
#5224=DIRECTION('',(1.,0.,0.));
#5225=DIRECTION('center_axis',(0.,1.,0.));
#5226=DIRECTION('ref_axis',(1.,0.,0.));
#5227=DIRECTION('center_axis',(0.,1.,0.));
#5228=DIRECTION('ref_axis',(1.,0.,0.));
#5229=DIRECTION('',(0.,1.,0.));
#5230=DIRECTION('center_axis',(0.,1.,0.));
#5231=DIRECTION('ref_axis',(1.,0.,0.));
#5232=DIRECTION('center_axis',(0.,1.,0.));
#5233=DIRECTION('ref_axis',(1.,0.,0.));
#5234=DIRECTION('center_axis',(0.,1.,0.));
#5235=DIRECTION('ref_axis',(1.,0.,0.));
#5236=DIRECTION('',(-1.,0.,0.));
#5237=DIRECTION('center_axis',(0.,1.,0.));
#5238=DIRECTION('ref_axis',(1.,0.,0.));
#5239=DIRECTION('center_axis',(0.,1.,0.));
#5240=DIRECTION('ref_axis',(1.,0.,0.));
#5241=DIRECTION('center_axis',(0.,1.,0.));
#5242=DIRECTION('ref_axis',(1.,0.,0.));
#5243=DIRECTION('',(0.,1.,0.));
#5244=DIRECTION('center_axis',(0.,1.,0.));
#5245=DIRECTION('ref_axis',(1.,0.,0.));
#5246=DIRECTION('center_axis',(0.,1.,0.));
#5247=DIRECTION('ref_axis',(1.,0.,0.));
#5248=DIRECTION('',(1.,0.,0.));
#5249=DIRECTION('center_axis',(0.,1.,0.));
#5250=DIRECTION('ref_axis',(1.,0.,0.));
#5251=DIRECTION('center_axis',(0.,1.,0.));
#5252=DIRECTION('ref_axis',(1.,0.,0.));
#5253=DIRECTION('',(0.,1.,0.));
#5254=DIRECTION('center_axis',(0.,1.,0.));
#5255=DIRECTION('ref_axis',(1.,0.,0.));
#5256=DIRECTION('center_axis',(0.,1.,0.));
#5257=DIRECTION('ref_axis',(1.,0.,0.));
#5258=DIRECTION('center_axis',(0.,1.,0.));
#5259=DIRECTION('ref_axis',(1.,0.,0.));
#5260=DIRECTION('',(-1.,0.,0.));
#5261=DIRECTION('center_axis',(0.,1.,0.));
#5262=DIRECTION('ref_axis',(1.,0.,0.));
#5263=DIRECTION('center_axis',(0.,1.,0.));
#5264=DIRECTION('ref_axis',(1.,0.,0.));
#5265=DIRECTION('center_axis',(0.,1.,0.));
#5266=DIRECTION('ref_axis',(1.,0.,0.));
#5267=DIRECTION('',(0.,1.,0.));
#5268=DIRECTION('center_axis',(0.,1.,0.));
#5269=DIRECTION('ref_axis',(1.,0.,0.));
#5270=DIRECTION('center_axis',(0.,1.,0.));
#5271=DIRECTION('ref_axis',(1.,0.,0.));
#5272=DIRECTION('',(1.,0.,0.));
#5273=DIRECTION('center_axis',(0.,1.,0.));
#5274=DIRECTION('ref_axis',(1.,0.,0.));
#5275=DIRECTION('center_axis',(0.,1.,0.));
#5276=DIRECTION('ref_axis',(1.,0.,0.));
#5277=DIRECTION('',(0.,1.,0.));
#5278=DIRECTION('center_axis',(0.,1.,0.));
#5279=DIRECTION('ref_axis',(1.,0.,0.));
#5280=DIRECTION('center_axis',(0.,1.,0.));
#5281=DIRECTION('ref_axis',(1.,0.,0.));
#5282=DIRECTION('center_axis',(1.,0.,0.));
#5283=DIRECTION('ref_axis',(0.,0.,-1.));
#5284=DIRECTION('center_axis',(1.,0.,0.));
#5285=DIRECTION('ref_axis',(0.,0.,-1.));
#5286=DIRECTION('',(1.,0.,0.));
#5287=DIRECTION('center_axis',(-1.,0.,0.));
#5288=DIRECTION('ref_axis',(0.,0.,-1.));
#5289=DIRECTION('center_axis',(1.,0.,0.));
#5290=DIRECTION('ref_axis',(0.,0.,-1.));
#5291=DIRECTION('center_axis',(1.,0.,0.));
#5292=DIRECTION('ref_axis',(0.,0.,-1.));
#5293=DIRECTION('center_axis',(1.,0.,0.));
#5294=DIRECTION('ref_axis',(0.,0.,-1.));
#5295=DIRECTION('center_axis',(1.,0.,0.));
#5296=DIRECTION('ref_axis',(0.,0.,-1.));
#5297=DIRECTION('',(1.,0.,0.));
#5298=DIRECTION('',(1.,0.,0.));
#5299=DIRECTION('',(1.,0.,0.));
#5300=DIRECTION('',(1.,0.,0.));
#5301=DIRECTION('center_axis',(0.,0.,1.));
#5302=DIRECTION('ref_axis',(1.,0.,0.));
#5303=DIRECTION('center_axis',(0.,0.,1.));
#5304=DIRECTION('ref_axis',(1.,0.,0.));
#5305=DIRECTION('',(0.,0.,1.));
#5306=DIRECTION('center_axis',(0.,0.,-1.));
#5307=DIRECTION('ref_axis',(1.,0.,0.));
#5308=DIRECTION('center_axis',(0.,0.,1.));
#5309=DIRECTION('ref_axis',(1.,0.,0.));
#5310=DIRECTION('center_axis',(0.,0.,1.));
#5311=DIRECTION('ref_axis',(1.,0.,0.));
#5312=DIRECTION('center_axis',(0.,0.,1.));
#5313=DIRECTION('ref_axis',(1.,0.,0.));
#5314=DIRECTION('center_axis',(0.,0.,1.));
#5315=DIRECTION('ref_axis',(1.,0.,0.));
#5316=DIRECTION('',(0.,0.,1.));
#5317=DIRECTION('center_axis',(0.,0.,-1.));
#5318=DIRECTION('ref_axis',(1.,0.,0.));
#5319=DIRECTION('center_axis',(0.,0.,1.));
#5320=DIRECTION('ref_axis',(1.,0.,0.));
#5321=DIRECTION('center_axis',(0.,0.,1.));
#5322=DIRECTION('ref_axis',(1.,0.,0.));
#5323=DIRECTION('center_axis',(0.,0.,1.));
#5324=DIRECTION('ref_axis',(1.,0.,0.));
#5325=DIRECTION('center_axis',(0.,0.,1.));
#5326=DIRECTION('ref_axis',(1.,0.,0.));
#5327=DIRECTION('',(0.,0.,1.));
#5328=DIRECTION('center_axis',(0.,0.,1.));
#5329=DIRECTION('ref_axis',(1.,0.,0.));
#5330=DIRECTION('center_axis',(0.,0.,1.));
#5331=DIRECTION('ref_axis',(1.,0.,0.));
#5332=DIRECTION('',(0.,0.,1.));
#5333=DIRECTION('center_axis',(0.,1.,0.));
#5334=DIRECTION('ref_axis',(-1.,0.,0.));
#5335=DIRECTION('',(-1.,0.,0.));
#5336=DIRECTION('',(0.,0.,1.));
#5337=DIRECTION('',(-1.,0.,0.));
#5338=DIRECTION('',(0.,0.,1.));
#5339=DIRECTION('center_axis',(1.,0.,0.));
#5340=DIRECTION('ref_axis',(0.,1.,0.));
#5341=DIRECTION('',(0.,1.,0.));
#5342=DIRECTION('',(0.,1.,0.));
#5343=DIRECTION('',(0.,0.,1.));
#5344=DIRECTION('center_axis',(0.,-1.,0.));
#5345=DIRECTION('ref_axis',(1.,0.,0.));
#5346=DIRECTION('',(1.,0.,0.));
#5347=DIRECTION('',(1.,0.,0.));
#5348=DIRECTION('',(0.,0.,1.));
#5349=DIRECTION('center_axis',(-1.,0.,0.));
#5350=DIRECTION('ref_axis',(0.,-1.,0.));
#5351=DIRECTION('',(0.,-1.,0.));
#5352=DIRECTION('',(0.,-1.,0.));
#5353=DIRECTION('center_axis',(0.,0.,1.));
#5354=DIRECTION('ref_axis',(1.,0.,0.));
#5355=DIRECTION('center_axis',(0.,0.,1.));
#5356=DIRECTION('ref_axis',(1.,0.,0.));
#5357=DIRECTION('axis',(0.,0.,1.));
#5358=DIRECTION('refdir',(1.,0.,0.));
#5359=DIRECTION('center_axis',(1.,0.,0.));
#5360=DIRECTION('ref_axis',(0.,0.,-1.));
#5361=DIRECTION('center_axis',(1.,0.,0.));
#5362=DIRECTION('ref_axis',(0.,0.,-1.));
#5363=DIRECTION('',(-1.,0.,0.));
#5364=DIRECTION('center_axis',(1.,0.,0.));
#5365=DIRECTION('ref_axis',(0.,0.,-1.));
#5366=DIRECTION('center_axis',(1.,0.,0.));
#5367=DIRECTION('ref_axis',(0.,0.,-1.));
#5368=DIRECTION('center_axis',(1.,0.,0.));
#5369=DIRECTION('ref_axis',(0.,0.,-1.));
#5370=DIRECTION('axis',(0.,0.,1.));
#5371=DIRECTION('refdir',(1.,0.,0.));
#5372=DIRECTION('center_axis',(0.,1.,0.));
#5373=DIRECTION('ref_axis',(1.,0.,0.));
#5374=DIRECTION('center_axis',(0.,1.,0.));
#5375=DIRECTION('ref_axis',(1.,0.,0.));
#5376=DIRECTION('',(0.,1.,0.));
#5377=DIRECTION('center_axis',(0.,-1.,0.));
#5378=DIRECTION('ref_axis',(1.,0.,0.));
#5379=DIRECTION('center_axis',(0.,1.,0.));
#5380=DIRECTION('ref_axis',(1.,0.,0.));
#5381=DIRECTION('center_axis',(0.,1.,0.));
#5382=DIRECTION('ref_axis',(1.,0.,0.));
#5383=DIRECTION('',(0.,1.,0.));
#5384=DIRECTION('center_axis',(0.,-1.,0.));
#5385=DIRECTION('ref_axis',(1.,0.,0.));
#5386=DIRECTION('center_axis',(0.,0.,1.));
#5387=DIRECTION('ref_axis',(1.,0.,0.));
#5388=DIRECTION('center_axis',(0.,1.,0.));
#5389=DIRECTION('ref_axis',(-1.,0.,0.));
#5390=DIRECTION('center_axis',(0.,1.,0.));
#5391=DIRECTION('ref_axis',(1.,0.,0.));
#5392=DIRECTION('center_axis',(0.,1.,0.));
#5393=DIRECTION('ref_axis',(1.,0.,0.));
#5394=DIRECTION('',(0.,-1.,0.));
#5395=DIRECTION('center_axis',(0.,-1.,0.));
#5396=DIRECTION('ref_axis',(1.,0.,0.));
#5397=DIRECTION('center_axis',(0.,1.,0.));
#5398=DIRECTION('ref_axis',(1.,0.,0.));
#5399=DIRECTION('center_axis',(0.,1.,0.));
#5400=DIRECTION('ref_axis',(1.,0.,0.));
#5401=DIRECTION('center_axis',(0.,1.,0.));
#5402=DIRECTION('ref_axis',(1.,0.,0.));
#5403=DIRECTION('',(0.,-1.,0.));
#5404=DIRECTION('center_axis',(0.,1.,0.));
#5405=DIRECTION('ref_axis',(1.,0.,0.));
#5406=DIRECTION('center_axis',(0.,1.,0.));
#5407=DIRECTION('ref_axis',(1.,0.,0.));
#5408=DIRECTION('center_axis',(0.,1.,0.));
#5409=DIRECTION('ref_axis',(1.,0.,0.));
#5410=DIRECTION('axis',(0.,0.,1.));
#5411=DIRECTION('refdir',(1.,0.,0.));
#5412=DIRECTION('center_axis',(0.,1.,0.));
#5413=DIRECTION('ref_axis',(1.,0.,0.));
#5414=DIRECTION('center_axis',(0.,1.,0.));
#5415=DIRECTION('ref_axis',(1.,0.,0.));
#5416=DIRECTION('',(0.,1.,0.));
#5417=DIRECTION('center_axis',(0.,-1.,0.));
#5418=DIRECTION('ref_axis',(1.,0.,0.));
#5419=DIRECTION('center_axis',(0.,1.,0.));
#5420=DIRECTION('ref_axis',(1.,0.,0.));
#5421=DIRECTION('center_axis',(0.,1.,0.));
#5422=DIRECTION('ref_axis',(1.,0.,0.));
#5423=DIRECTION('',(0.,1.,0.));
#5424=DIRECTION('center_axis',(0.,-1.,0.));
#5425=DIRECTION('ref_axis',(1.,0.,0.));
#5426=DIRECTION('center_axis',(6.12323399573677E-17,0.,1.));
#5427=DIRECTION('ref_axis',(1.,0.,0.));
#5428=DIRECTION('center_axis',(0.,1.,0.));
#5429=DIRECTION('ref_axis',(-1.,0.,0.));
#5430=DIRECTION('center_axis',(0.,1.,0.));
#5431=DIRECTION('ref_axis',(1.,0.,0.));
#5432=DIRECTION('center_axis',(0.,1.,0.));
#5433=DIRECTION('ref_axis',(1.,0.,0.));
#5434=DIRECTION('',(0.,-1.,0.));
#5435=DIRECTION('center_axis',(0.,-1.,0.));
#5436=DIRECTION('ref_axis',(1.,0.,0.));
#5437=DIRECTION('center_axis',(0.,1.,0.));
#5438=DIRECTION('ref_axis',(1.,0.,0.));
#5439=DIRECTION('center_axis',(0.,1.,0.));
#5440=DIRECTION('ref_axis',(1.,0.,0.));
#5441=DIRECTION('center_axis',(0.,1.,0.));
#5442=DIRECTION('ref_axis',(1.,0.,0.));
#5443=DIRECTION('',(0.,-1.,0.));
#5444=DIRECTION('center_axis',(0.,1.,0.));
#5445=DIRECTION('ref_axis',(1.,0.,0.));
#5446=DIRECTION('center_axis',(0.,1.,0.));
#5447=DIRECTION('ref_axis',(1.,0.,0.));
#5448=DIRECTION('center_axis',(0.,1.,0.));
#5449=DIRECTION('ref_axis',(1.,0.,0.));
#5450=DIRECTION('axis',(0.,0.,1.));
#5451=DIRECTION('refdir',(1.,0.,0.));
#5452=DIRECTION('center_axis',(0.,1.,0.));
#5453=DIRECTION('ref_axis',(1.,0.,0.));
#5454=DIRECTION('center_axis',(0.,1.,0.));
#5455=DIRECTION('ref_axis',(1.,0.,0.));
#5456=DIRECTION('',(0.,1.,0.));
#5457=DIRECTION('center_axis',(0.,-1.,0.));
#5458=DIRECTION('ref_axis',(1.,0.,0.));
#5459=DIRECTION('center_axis',(0.,1.,0.));
#5460=DIRECTION('ref_axis',(1.,0.,0.));
#5461=DIRECTION('center_axis',(0.,1.,0.));
#5462=DIRECTION('ref_axis',(1.,0.,0.));
#5463=DIRECTION('',(0.,1.,0.));
#5464=DIRECTION('center_axis',(0.,-1.,0.));
#5465=DIRECTION('ref_axis',(1.,0.,0.));
#5466=DIRECTION('center_axis',(0.,0.,1.));
#5467=DIRECTION('ref_axis',(1.,0.,0.));
#5468=DIRECTION('center_axis',(0.,1.,0.));
#5469=DIRECTION('ref_axis',(-1.,0.,0.));
#5470=DIRECTION('center_axis',(0.,1.,0.));
#5471=DIRECTION('ref_axis',(1.,0.,0.));
#5472=DIRECTION('center_axis',(0.,1.,0.));
#5473=DIRECTION('ref_axis',(1.,0.,0.));
#5474=DIRECTION('',(0.,-1.,0.));
#5475=DIRECTION('center_axis',(0.,-1.,0.));
#5476=DIRECTION('ref_axis',(1.,0.,0.));
#5477=DIRECTION('center_axis',(0.,1.,0.));
#5478=DIRECTION('ref_axis',(1.,0.,0.));
#5479=DIRECTION('center_axis',(0.,1.,0.));
#5480=DIRECTION('ref_axis',(1.,0.,0.));
#5481=DIRECTION('center_axis',(0.,1.,0.));
#5482=DIRECTION('ref_axis',(1.,0.,0.));
#5483=DIRECTION('',(0.,-1.,0.));
#5484=DIRECTION('center_axis',(0.,1.,0.));
#5485=DIRECTION('ref_axis',(1.,0.,0.));
#5486=DIRECTION('center_axis',(0.,1.,0.));
#5487=DIRECTION('ref_axis',(1.,0.,0.));
#5488=DIRECTION('center_axis',(0.,1.,0.));
#5489=DIRECTION('ref_axis',(1.,0.,0.));
#5490=DIRECTION('axis',(0.,0.,1.));
#5491=DIRECTION('refdir',(1.,0.,0.));
#5492=DIRECTION('center_axis',(0.,0.,-1.));
#5493=DIRECTION('ref_axis',(0.,1.,0.));
#5494=DIRECTION('',(0.,1.,0.));
#5495=DIRECTION('',(1.,0.,0.));
#5496=DIRECTION('',(0.,-1.,0.));
#5497=DIRECTION('',(1.,0.,0.));
#5498=DIRECTION('center_axis',(0.,1.,-8.88178419700125E-16));
#5499=DIRECTION('ref_axis',(0.,8.88178419700125E-16,1.));
#5500=DIRECTION('',(0.,8.88178419700125E-16,1.));
#5501=DIRECTION('',(1.,0.,0.));
#5502=DIRECTION('',(0.,-8.88178419700125E-16,-1.));
#5503=DIRECTION('center_axis',(0.,-7.40148683083439E-16,-1.));
#5504=DIRECTION('ref_axis',(0.,1.,-7.40148683083439E-16));
#5505=DIRECTION('',(0.,1.,-7.40148683083439E-16));
#5506=DIRECTION('',(1.,0.,0.));
#5507=DIRECTION('',(0.,-1.,7.40148683083439E-16));
#5508=DIRECTION('center_axis',(0.,-0.707106781186547,-0.707106781186548));
#5509=DIRECTION('ref_axis',(0.,0.707106781186548,-0.707106781186547));
#5510=DIRECTION('',(0.,0.707106781186548,-0.707106781186547));
#5511=DIRECTION('',(1.,0.,0.));
#5512=DIRECTION('',(0.,-0.707106781186548,0.707106781186547));
#5513=DIRECTION('center_axis',(0.,-1.,2.77555756156289E-16));
#5514=DIRECTION('ref_axis',(0.,-2.77555756156289E-16,-1.));
#5515=DIRECTION('',(0.,-2.77555756156289E-16,-1.));
#5516=DIRECTION('',(1.,0.,0.));
#5517=DIRECTION('',(0.,2.77555756156289E-16,1.));
#5518=DIRECTION('center_axis',(0.,-0.707106781186547,0.707106781186548));
#5519=DIRECTION('ref_axis',(0.,-0.707106781186548,-0.707106781186547));
#5520=DIRECTION('',(0.,-0.707106781186548,-0.707106781186547));
#5521=DIRECTION('',(1.,0.,0.));
#5522=DIRECTION('',(0.,0.707106781186548,0.707106781186547));
#5523=DIRECTION('center_axis',(0.,7.40148683083438E-16,1.));
#5524=DIRECTION('ref_axis',(0.,-1.,7.40148683083438E-16));
#5525=DIRECTION('',(0.,-1.,7.40148683083438E-16));
#5526=DIRECTION('',(1.,0.,0.));
#5527=DIRECTION('',(0.,1.,-7.40148683083438E-16));
#5528=DIRECTION('center_axis',(0.,1.,-4.44089209850063E-16));
#5529=DIRECTION('ref_axis',(0.,4.44089209850063E-16,1.));
#5530=DIRECTION('',(0.,4.44089209850063E-16,1.));
#5531=DIRECTION('',(1.,0.,0.));
#5532=DIRECTION('',(0.,-4.44089209850063E-16,-1.));
#5533=DIRECTION('center_axis',(0.,2.41352831440251E-16,1.));
#5534=DIRECTION('ref_axis',(0.,-1.,2.41352831440251E-16));
#5535=DIRECTION('',(0.,-1.,2.41352831440251E-16));
#5536=DIRECTION('',(-1.,0.,0.));
#5537=DIRECTION('',(0.,1.,-2.41352831440251E-16));
#5538=DIRECTION('center_axis',(0.,-1.,2.41352831440251E-16));
#5539=DIRECTION('ref_axis',(0.,-2.41352831440251E-16,-1.));
#5540=DIRECTION('',(0.,-2.41352831440251E-16,-1.));
#5541=DIRECTION('',(1.,0.,0.));
#5542=DIRECTION('',(0.,2.41352831440251E-16,1.));
#5543=DIRECTION('',(1.,0.,0.));
#5544=DIRECTION('center_axis',(0.,0.,-1.));
#5545=DIRECTION('ref_axis',(0.,1.,0.));
#5546=DIRECTION('',(0.,1.,0.));
#5547=DIRECTION('',(1.,0.,0.));
#5548=DIRECTION('',(0.,-1.,0.));
#5549=DIRECTION('center_axis',(0.,-1.,0.));
#5550=DIRECTION('ref_axis',(0.,0.,-1.));
#5551=DIRECTION('',(0.,0.,-1.));
#5552=DIRECTION('',(1.,0.,0.));
#5553=DIRECTION('',(0.,0.,1.));
#5554=DIRECTION('center_axis',(0.,-0.707106781186547,0.707106781186548));
#5555=DIRECTION('ref_axis',(0.,-0.707106781186548,-0.707106781186547));
#5556=DIRECTION('',(0.,-0.707106781186548,-0.707106781186547));
#5557=DIRECTION('',(1.,0.,0.));
#5558=DIRECTION('',(0.,0.707106781186548,0.707106781186547));
#5559=DIRECTION('center_axis',(0.,0.,1.));
#5560=DIRECTION('ref_axis',(0.,-1.,0.));
#5561=DIRECTION('',(0.,-1.,0.));
#5562=DIRECTION('',(1.,0.,0.));
#5563=DIRECTION('',(0.,1.,0.));
#5564=DIRECTION('center_axis',(0.,0.707106781186548,0.707106781186547));
#5565=DIRECTION('ref_axis',(0.,-0.707106781186547,0.707106781186548));
#5566=DIRECTION('',(0.,-0.707106781186547,0.707106781186548));
#5567=DIRECTION('',(1.,0.,0.));
#5568=DIRECTION('',(0.,0.707106781186547,-0.707106781186548));
#5569=DIRECTION('center_axis',(0.,1.,0.));
#5570=DIRECTION('ref_axis',(0.,0.,1.));
#5571=DIRECTION('',(0.,0.,1.));
#5572=DIRECTION('',(1.,0.,0.));
#5573=DIRECTION('',(0.,0.,-1.));
#5574=DIRECTION('center_axis',(0.,0.,-1.));
#5575=DIRECTION('ref_axis',(0.,1.,0.));
#5576=DIRECTION('',(0.,1.,0.));
#5577=DIRECTION('',(1.,0.,0.));
#5578=DIRECTION('',(0.,-1.,0.));
#5579=DIRECTION('center_axis',(0.,1.,-2.41352831440251E-16));
#5580=DIRECTION('ref_axis',(0.,2.41352831440251E-16,1.));
#5581=DIRECTION('',(0.,2.41352831440251E-16,1.));
#5582=DIRECTION('',(-1.,0.,0.));
#5583=DIRECTION('',(0.,-2.41352831440251E-16,-1.));
#5584=DIRECTION('center_axis',(0.,0.,1.));
#5585=DIRECTION('ref_axis',(0.,-1.,0.));
#5586=DIRECTION('',(0.,-1.,0.));
#5587=DIRECTION('',(1.,0.,0.));
#5588=DIRECTION('',(0.,1.,0.));
#5589=DIRECTION('',(1.,0.,0.));
#5590=DIRECTION('center_axis',(0.,-1.,0.));
#5591=DIRECTION('ref_axis',(0.,0.,-1.));
#5592=DIRECTION('',(0.,0.,-1.));
#5593=DIRECTION('',(1.,0.,0.));
#5594=DIRECTION('',(0.,0.,1.));
#5595=DIRECTION('center_axis',(0.,0.,1.));
#5596=DIRECTION('ref_axis',(0.,-1.,0.));
#5597=DIRECTION('',(0.,-1.,0.));
#5598=DIRECTION('',(1.,0.,0.));
#5599=DIRECTION('',(0.,1.,0.));
#5600=DIRECTION('center_axis',(0.,0.707106781186548,0.707106781186548));
#5601=DIRECTION('ref_axis',(0.,-0.707106781186548,0.707106781186548));
#5602=DIRECTION('',(0.,-0.707106781186548,0.707106781186548));
#5603=DIRECTION('',(1.,0.,0.));
#5604=DIRECTION('',(0.,0.707106781186548,-0.707106781186548));
#5605=DIRECTION('center_axis',(0.,1.,0.));
#5606=DIRECTION('ref_axis',(0.,0.,1.));
#5607=DIRECTION('',(0.,0.,1.));
#5608=DIRECTION('',(1.,0.,0.));
#5609=DIRECTION('',(0.,0.,-1.));
#5610=DIRECTION('center_axis',(0.,0.707106781186548,-0.707106781186547));
#5611=DIRECTION('ref_axis',(0.,0.707106781186547,0.707106781186548));
#5612=DIRECTION('',(0.,0.707106781186547,0.707106781186548));
#5613=DIRECTION('',(1.,0.,0.));
#5614=DIRECTION('',(0.,-0.707106781186547,-0.707106781186548));
#5615=DIRECTION('center_axis',(0.,-7.40148683083438E-16,-1.));
#5616=DIRECTION('ref_axis',(0.,1.,-7.40148683083438E-16));
#5617=DIRECTION('',(0.,1.,-7.40148683083438E-16));
#5618=DIRECTION('',(1.,0.,0.));
#5619=DIRECTION('',(0.,-1.,7.40148683083438E-16));
#5620=DIRECTION('center_axis',(0.,-1.,0.));
#5621=DIRECTION('ref_axis',(0.,0.,-1.));
#5622=DIRECTION('',(0.,0.,-1.));
#5623=DIRECTION('',(1.,0.,0.));
#5624=DIRECTION('',(0.,0.,1.));
#5625=DIRECTION('center_axis',(0.,0.,-1.));
#5626=DIRECTION('ref_axis',(0.,1.,0.));
#5627=DIRECTION('',(0.,1.,0.));
#5628=DIRECTION('',(-1.,0.,0.));
#5629=DIRECTION('',(0.,-1.,0.));
#5630=DIRECTION('center_axis',(0.,1.,0.));
#5631=DIRECTION('ref_axis',(0.,0.,1.));
#5632=DIRECTION('',(0.,0.,1.));
#5633=DIRECTION('',(1.,0.,0.));
#5634=DIRECTION('',(0.,0.,-1.));
#5635=DIRECTION('',(1.,0.,0.));
#5636=DIRECTION('center_axis',(0.,0.,1.));
#5637=DIRECTION('ref_axis',(0.,-1.,0.));
#5638=DIRECTION('',(0.,-1.,0.));
#5639=DIRECTION('',(1.,0.,0.));
#5640=DIRECTION('',(0.,1.,0.));
#5641=DIRECTION('center_axis',(0.,1.,0.));
#5642=DIRECTION('ref_axis',(0.,0.,1.));
#5643=DIRECTION('',(0.,0.,1.));
#5644=DIRECTION('',(1.,0.,0.));
#5645=DIRECTION('',(0.,0.,-1.));
#5646=DIRECTION('center_axis',(0.,0.707106781186547,-0.707106781186548));
#5647=DIRECTION('ref_axis',(0.,0.707106781186548,0.707106781186547));
#5648=DIRECTION('',(0.,0.707106781186548,0.707106781186547));
#5649=DIRECTION('',(1.,0.,0.));
#5650=DIRECTION('',(0.,-0.707106781186548,-0.707106781186547));
#5651=DIRECTION('center_axis',(0.,0.,-1.));
#5652=DIRECTION('ref_axis',(0.,1.,0.));
#5653=DIRECTION('',(0.,1.,0.));
#5654=DIRECTION('',(1.,0.,0.));
#5655=DIRECTION('',(0.,-1.,0.));
#5656=DIRECTION('center_axis',(0.,-0.707106781186547,-0.707106781186548));
#5657=DIRECTION('ref_axis',(0.,0.707106781186548,-0.707106781186547));
#5658=DIRECTION('',(0.,0.707106781186548,-0.707106781186547));
#5659=DIRECTION('',(1.,0.,0.));
#5660=DIRECTION('',(0.,-0.707106781186548,0.707106781186547));
#5661=DIRECTION('center_axis',(0.,-1.,0.));
#5662=DIRECTION('ref_axis',(0.,0.,-1.));
#5663=DIRECTION('',(0.,0.,-1.));
#5664=DIRECTION('',(1.,0.,0.));
#5665=DIRECTION('',(0.,0.,1.));
#5666=DIRECTION('center_axis',(0.,0.,1.));
#5667=DIRECTION('ref_axis',(0.,-1.,0.));
#5668=DIRECTION('',(0.,-1.,0.));
#5669=DIRECTION('',(1.,0.,0.));
#5670=DIRECTION('',(0.,1.,0.));
#5671=DIRECTION('center_axis',(0.,-1.,0.));
#5672=DIRECTION('ref_axis',(0.,0.,-1.));
#5673=DIRECTION('',(0.,0.,-1.));
#5674=DIRECTION('',(-1.,0.,0.));
#5675=DIRECTION('',(0.,0.,1.));
#5676=DIRECTION('center_axis',(1.,0.,0.));
#5677=DIRECTION('ref_axis',(0.,0.,-1.));
#5678=DIRECTION('center_axis',(1.,0.,0.));
#5679=DIRECTION('ref_axis',(0.,0.,-1.));
#5680=DIRECTION('',(1.,0.,0.));
#5681=DIRECTION('center_axis',(-1.,0.,0.));
#5682=DIRECTION('ref_axis',(0.,0.,-1.));
#5683=DIRECTION('center_axis',(0.,1.,0.));
#5684=DIRECTION('ref_axis',(0.,0.,1.));
#5685=DIRECTION('',(0.,0.,1.));
#5686=DIRECTION('',(1.,0.,0.));
#5687=DIRECTION('',(0.,0.,1.));
#5688=DIRECTION('center_axis',(0.,1.,0.));
#5689=DIRECTION('ref_axis',(0.,0.,1.));
#5690=DIRECTION('',(0.,0.,1.));
#5691=DIRECTION('',(1.,0.,0.));
#5692=DIRECTION('',(0.,0.,1.));
#5693=DIRECTION('center_axis',(0.,0.,-1.));
#5694=DIRECTION('ref_axis',(0.,1.,0.));
#5695=DIRECTION('',(0.,1.,0.));
#5696=DIRECTION('',(0.,1.,0.));
#5697=DIRECTION('center_axis',(0.,0.,-1.));
#5698=DIRECTION('ref_axis',(0.,1.,0.));
#5699=DIRECTION('',(0.,1.,0.));
#5700=DIRECTION('',(1.,0.,0.));
#5701=DIRECTION('',(0.,1.,0.));
#5702=DIRECTION('center_axis',(0.,-1.,0.));
#5703=DIRECTION('ref_axis',(0.,0.,-1.));
#5704=DIRECTION('',(0.,0.,-1.));
#5705=DIRECTION('',(0.,0.,-1.));
#5706=DIRECTION('center_axis',(0.,-1.,0.));
#5707=DIRECTION('ref_axis',(0.,0.,-1.));
#5708=DIRECTION('',(0.,0.,-1.));
#5709=DIRECTION('',(1.,0.,0.));
#5710=DIRECTION('',(0.,0.,-1.));
#5711=DIRECTION('center_axis',(0.,0.,1.));
#5712=DIRECTION('ref_axis',(0.,-1.,0.));
#5713=DIRECTION('',(0.,-1.,0.));
#5714=DIRECTION('',(0.,-1.,0.));
#5715=DIRECTION('center_axis',(0.,0.,1.));
#5716=DIRECTION('ref_axis',(0.,-1.,0.));
#5717=DIRECTION('',(0.,-1.,0.));
#5718=DIRECTION('',(0.,-1.,0.));
#5719=DIRECTION('center_axis',(1.,0.,0.));
#5720=DIRECTION('ref_axis',(0.,0.,-1.));
#5721=DIRECTION('center_axis',(1.,0.,0.));
#5722=DIRECTION('ref_axis',(0.,0.,-1.));
#5723=DIRECTION('axis',(0.,0.,1.));
#5724=DIRECTION('refdir',(1.,0.,0.));
#5725=DIRECTION('center_axis',(0.,1.,0.));
#5726=DIRECTION('ref_axis',(1.,0.,0.));
#5727=DIRECTION('center_axis',(0.,1.,0.));
#5728=DIRECTION('ref_axis',(1.,0.,0.));
#5729=DIRECTION('',(0.707106781186548,-0.707106781186547,-8.65956056235494E-17));
#5730=DIRECTION('center_axis',(0.,-1.,0.));
#5731=DIRECTION('ref_axis',(1.,0.,0.));
#5732=DIRECTION('center_axis',(0.,1.,0.));
#5733=DIRECTION('ref_axis',(1.,0.,0.));
#5734=DIRECTION('',(0.,-1.,0.));
#5735=DIRECTION('center_axis',(0.,-1.,0.));
#5736=DIRECTION('ref_axis',(1.,0.,0.));
#5737=DIRECTION('center_axis',(0.,1.,0.));
#5738=DIRECTION('ref_axis',(1.,0.,0.));
#5739=DIRECTION('center_axis',(0.,1.,0.));
#5740=DIRECTION('ref_axis',(1.,0.,0.));
#5741=DIRECTION('center_axis',(0.,1.,0.));
#5742=DIRECTION('ref_axis',(1.,0.,0.));
#5743=DIRECTION('',(0.,-1.,0.));
#5744=DIRECTION('center_axis',(0.,1.,0.));
#5745=DIRECTION('ref_axis',(1.,0.,0.));
#5746=DIRECTION('center_axis',(0.,1.,0.));
#5747=DIRECTION('ref_axis',(1.,0.,0.));
#5748=DIRECTION('axis',(0.,0.,1.));
#5749=DIRECTION('refdir',(1.,0.,0.));
#5750=DIRECTION('center_axis',(0.866025403784439,0.,-0.5));
#5751=DIRECTION('ref_axis',(0.5,0.,0.866025403784439));
#5752=DIRECTION('',(-0.5,0.,-0.866025403784439));
#5753=DIRECTION('',(0.,-1.,0.));
#5754=DIRECTION('',(0.5,0.,0.866025403784439));
#5755=DIRECTION('',(0.,-1.,0.));
#5756=DIRECTION('center_axis',(1.20185167898973E-16,0.,-1.));
#5757=DIRECTION('ref_axis',(1.,0.,1.20185167898973E-16));
#5758=DIRECTION('',(-1.,0.,-1.20185167898973E-16));
#5759=DIRECTION('',(0.,-1.,0.));
#5760=DIRECTION('',(1.,0.,1.20185167898973E-16));
#5761=DIRECTION('center_axis',(-0.866025403784439,0.,-0.5));
#5762=DIRECTION('ref_axis',(0.5,0.,-0.866025403784439));
#5763=DIRECTION('',(-0.5,0.,0.866025403784439));
#5764=DIRECTION('',(0.,-1.,0.));
#5765=DIRECTION('',(0.5,0.,-0.866025403784439));
#5766=DIRECTION('center_axis',(-0.866025403784439,0.,0.5));
#5767=DIRECTION('ref_axis',(-0.5,0.,-0.866025403784439));
#5768=DIRECTION('',(0.5,0.,0.866025403784439));
#5769=DIRECTION('',(0.,-1.,0.));
#5770=DIRECTION('',(-0.5,0.,-0.866025403784439));
#5771=DIRECTION('center_axis',(-2.40370335797945E-16,0.,1.));
#5772=DIRECTION('ref_axis',(-1.,0.,-2.40370335797945E-16));
#5773=DIRECTION('',(1.,0.,2.40370335797945E-16));
#5774=DIRECTION('',(0.,-1.,0.));
#5775=DIRECTION('',(-1.,0.,-2.40370335797945E-16));
#5776=DIRECTION('center_axis',(0.866025403784439,0.,0.5));
#5777=DIRECTION('ref_axis',(-0.5,0.,0.866025403784439));
#5778=DIRECTION('',(0.5,0.,-0.866025403784439));
#5779=DIRECTION('',(-0.5,0.,0.866025403784439));
#5780=DIRECTION('center_axis',(0.,1.,0.));
#5781=DIRECTION('ref_axis',(1.,0.,0.));
#5782=DIRECTION('center_axis',(0.,-1.,0.));
#5783=DIRECTION('ref_axis',(0.,0.,-1.));
#5784=DIRECTION('center_axis',(0.,1.,0.));
#5785=DIRECTION('ref_axis',(1.,0.,0.));
#5786=DIRECTION('center_axis',(0.,1.,0.));
#5787=DIRECTION('ref_axis',(1.,0.,0.));
#5788=DIRECTION('center_axis',(0.,1.,0.));
#5789=DIRECTION('ref_axis',(0.,0.,1.));
#5790=DIRECTION('center_axis',(0.,-1.,0.));
#5791=DIRECTION('ref_axis',(1.,0.,0.));
#5792=DIRECTION('center_axis',(0.,-1.,0.));
#5793=DIRECTION('ref_axis',(1.,0.,0.));
#5794=DIRECTION('center_axis',(0.,-1.,0.));
#5795=DIRECTION('ref_axis',(1.,0.,0.));
#5796=DIRECTION('',(0.707106781186548,0.707106781186547,8.65956056235493E-17));
#5797=DIRECTION('center_axis',(0.,-1.,0.));
#5798=DIRECTION('ref_axis',(1.,0.,0.));
#5799=DIRECTION('center_axis',(0.,-1.,0.));
#5800=DIRECTION('ref_axis',(1.,0.,0.));
#5801=DIRECTION('',(0.,1.,0.));
#5802=DIRECTION('center_axis',(0.,1.,0.));
#5803=DIRECTION('ref_axis',(1.,0.,0.));
#5804=DIRECTION('center_axis',(0.,-1.,0.));
#5805=DIRECTION('ref_axis',(1.,0.,0.));
#5806=DIRECTION('',(-0.707106781186547,0.707106781186548,-8.65956056235493E-17));
#5807=DIRECTION('center_axis',(0.,-1.,0.));
#5808=DIRECTION('ref_axis',(0.,0.,-1.));
#5809=DIRECTION('center_axis',(0.,-1.,0.));
#5810=DIRECTION('ref_axis',(1.,0.,0.));
#5811=DIRECTION('center_axis',(0.,1.,0.));
#5812=DIRECTION('ref_axis',(1.,0.,0.));
#5813=DIRECTION('center_axis',(0.,1.,0.));
#5814=DIRECTION('ref_axis',(1.,0.,0.));
#5815=DIRECTION('',(-0.447213595499958,0.894427190999916,-5.47678698264203E-17));
#5816=DIRECTION('center_axis',(0.,-1.,0.));
#5817=DIRECTION('ref_axis',(1.,0.,0.));
#5818=DIRECTION('',(0.,1.,0.));
#5819=DIRECTION('axis',(0.,0.,1.));
#5820=DIRECTION('refdir',(1.,0.,0.));
#5821=DIRECTION('center_axis',(0.,1.,0.));
#5822=DIRECTION('ref_axis',(0.,0.,1.));
#5823=DIRECTION('center_axis',(0.,-1.,0.));
#5824=DIRECTION('ref_axis',(1.,0.,0.));
#5825=DIRECTION('center_axis',(0.,-1.,0.));
#5826=DIRECTION('ref_axis',(1.,0.,0.));
#5827=DIRECTION('center_axis',(0.,-1.,0.));
#5828=DIRECTION('ref_axis',(1.,0.,0.));
#5829=DIRECTION('',(0.707106781186547,0.707106781186548,8.65956056235493E-17));
#5830=DIRECTION('center_axis',(0.,-1.,0.));
#5831=DIRECTION('ref_axis',(1.,0.,0.));
#5832=DIRECTION('center_axis',(0.,-1.,0.));
#5833=DIRECTION('ref_axis',(1.,0.,0.));
#5834=DIRECTION('',(0.,1.,0.));
#5835=DIRECTION('center_axis',(0.,1.,0.));
#5836=DIRECTION('ref_axis',(1.,0.,0.));
#5837=DIRECTION('center_axis',(0.,-1.,0.));
#5838=DIRECTION('ref_axis',(1.,0.,0.));
#5839=DIRECTION('',(-0.707106781186547,0.707106781186548,-8.65956056235493E-17));
#5840=DIRECTION('center_axis',(0.,-1.,0.));
#5841=DIRECTION('ref_axis',(0.,0.,-1.));
#5842=DIRECTION('center_axis',(0.,-1.,0.));
#5843=DIRECTION('ref_axis',(1.,0.,0.));
#5844=DIRECTION('center_axis',(0.,1.,0.));
#5845=DIRECTION('ref_axis',(1.,0.,0.));
#5846=DIRECTION('center_axis',(0.,1.,0.));
#5847=DIRECTION('ref_axis',(1.,0.,0.));
#5848=DIRECTION('',(-0.447213595499958,0.894427190999916,-5.47678698264203E-17));
#5849=DIRECTION('center_axis',(0.,-1.,0.));
#5850=DIRECTION('ref_axis',(1.,0.,0.));
#5851=DIRECTION('center_axis',(0.,1.,0.));
#5852=DIRECTION('ref_axis',(1.,0.,0.));
#5853=DIRECTION('',(0.,1.,0.));
#5854=DIRECTION('center_axis',(0.,1.,0.));
#5855=DIRECTION('ref_axis',(1.,0.,0.));
#5856=DIRECTION('center_axis',(0.,-1.,0.));
#5857=DIRECTION('ref_axis',(1.,0.,0.));
#5858=DIRECTION('',(-0.707106781186547,0.707106781186548,-8.65956056235493E-17));
#5859=DIRECTION('center_axis',(0.,-1.,0.));
#5860=DIRECTION('ref_axis',(0.,0.,-1.));
#5861=DIRECTION('center_axis',(0.866025403784439,0.,-0.5));
#5862=DIRECTION('ref_axis',(0.5,0.,0.866025403784439));
#5863=DIRECTION('',(-0.5,0.,-0.866025403784439));
#5864=DIRECTION('',(0.,-1.,0.));
#5865=DIRECTION('',(0.5,0.,0.866025403784439));
#5866=DIRECTION('',(0.,-1.,0.));
#5867=DIRECTION('center_axis',(1.60246890531964E-16,0.,-1.));
#5868=DIRECTION('ref_axis',(1.,0.,1.60246890531964E-16));
#5869=DIRECTION('',(-1.,0.,-1.60246890531964E-16));
#5870=DIRECTION('',(0.,-1.,0.));
#5871=DIRECTION('',(1.,0.,1.60246890531964E-16));
#5872=DIRECTION('center_axis',(-0.866025403784439,0.,-0.5));
#5873=DIRECTION('ref_axis',(0.5,0.,-0.866025403784439));
#5874=DIRECTION('',(-0.5,0.,0.866025403784439));
#5875=DIRECTION('',(0.,-1.,0.));
#5876=DIRECTION('',(0.5,0.,-0.866025403784439));
#5877=DIRECTION('center_axis',(-0.866025403784439,0.,0.5));
#5878=DIRECTION('ref_axis',(-0.5,0.,-0.866025403784439));
#5879=DIRECTION('',(0.5,0.,0.866025403784439));
#5880=DIRECTION('',(0.,-1.,0.));
#5881=DIRECTION('',(-0.5,0.,-0.866025403784439));
#5882=DIRECTION('center_axis',(-1.60246890531964E-16,0.,1.));
#5883=DIRECTION('ref_axis',(-1.,0.,-1.60246890531964E-16));
#5884=DIRECTION('',(1.,0.,1.60246890531964E-16));
#5885=DIRECTION('',(0.,-1.,0.));
#5886=DIRECTION('',(-1.,0.,-1.60246890531964E-16));
#5887=DIRECTION('center_axis',(0.866025403784439,0.,0.5));
#5888=DIRECTION('ref_axis',(-0.5,0.,0.866025403784439));
#5889=DIRECTION('',(0.5,0.,-0.866025403784439));
#5890=DIRECTION('',(-0.5,0.,0.866025403784439));
#5891=DIRECTION('center_axis',(0.,1.,0.));
#5892=DIRECTION('ref_axis',(1.,0.,0.));
#5893=DIRECTION('center_axis',(0.,-1.,0.));
#5894=DIRECTION('ref_axis',(0.,0.,-1.));
#5895=DIRECTION('axis',(0.,0.,1.));
#5896=DIRECTION('refdir',(1.,0.,0.));
#5897=DIRECTION('center_axis',(0.,1.,0.));
#5898=DIRECTION('ref_axis',(1.,0.,0.));
#5899=DIRECTION('',(-0.5,0.,0.866025403784439));
#5900=DIRECTION('',(-1.,0.,-3.29650746237182E-16));
#5901=DIRECTION('',(-0.5,0.,-0.866025403784439));
#5902=DIRECTION('',(0.5,0.,-0.866025403784438));
#5903=DIRECTION('',(1.,0.,0.));
#5904=DIRECTION('',(0.5,0.,0.866025403784439));
#5905=DIRECTION('center_axis',(0.,-1.,0.));
#5906=DIRECTION('ref_axis',(1.,0.,0.));
#5907=DIRECTION('center_axis',(0.,1.,0.));
#5908=DIRECTION('ref_axis',(1.,0.,0.));
#5909=DIRECTION('',(0.5,0.,-0.866025403784439));
#5910=DIRECTION('',(-0.5,0.,-0.866025403784439));
#5911=DIRECTION('',(-1.,0.,0.));
#5912=DIRECTION('',(-0.5,0.,0.866025403784438));
#5913=DIRECTION('',(0.5,0.,0.866025403784439));
#5914=DIRECTION('',(1.,0.,3.29650746237182E-16));
#5915=DIRECTION('center_axis',(0.,1.,0.));
#5916=DIRECTION('ref_axis',(1.,0.,0.));
#5917=DIRECTION('center_axis',(-3.29650746237182E-16,0.,1.));
#5918=DIRECTION('ref_axis',(1.,0.,3.29650746237182E-16));
#5919=DIRECTION('',(0.,-1.,0.));
#5920=DIRECTION('',(0.,1.,0.));
#5921=DIRECTION('center_axis',(-0.866025403784439,0.,0.5));
#5922=DIRECTION('ref_axis',(0.5,0.,0.866025403784439));
#5923=DIRECTION('',(0.,1.,0.));
#5924=DIRECTION('center_axis',(-0.866025403784439,0.,-0.5));
#5925=DIRECTION('ref_axis',(-0.5,0.,0.866025403784439));
#5926=DIRECTION('',(0.,1.,0.));
#5927=DIRECTION('center_axis',(0.,0.,-1.));
#5928=DIRECTION('ref_axis',(-1.,0.,0.));
#5929=DIRECTION('',(0.,1.,0.));
#5930=DIRECTION('center_axis',(0.866025403784439,0.,-0.5));
#5931=DIRECTION('ref_axis',(-0.5,0.,-0.866025403784439));
#5932=DIRECTION('',(0.,1.,0.));
#5933=DIRECTION('center_axis',(0.866025403784439,0.,0.5));
#5934=DIRECTION('ref_axis',(0.5,0.,-0.866025403784439));
#5935=DIRECTION('center_axis',(0.,-1.,0.));
#5936=DIRECTION('ref_axis',(1.,0.,0.));
#5937=DIRECTION('',(0.,1.,0.));
#5938=DIRECTION('center_axis',(0.,-1.,0.));
#5939=DIRECTION('ref_axis',(1.,0.,0.));
#5940=DIRECTION('center_axis',(0.,1.,0.));
#5941=DIRECTION('ref_axis',(0.,0.,1.));
#5942=DIRECTION('center_axis',(0.,-1.,0.));
#5943=DIRECTION('ref_axis',(1.,0.,0.));
#5944=DIRECTION('center_axis',(0.,-1.,0.));
#5945=DIRECTION('ref_axis',(1.,0.,0.));
#5946=DIRECTION('center_axis',(0.,-1.,0.));
#5947=DIRECTION('ref_axis',(1.,0.,0.));
#5948=DIRECTION('',(0.707106781186547,0.707106781186548,8.65956056235493E-17));
#5949=DIRECTION('center_axis',(0.,-1.,0.));
#5950=DIRECTION('ref_axis',(1.,0.,0.));
#5951=DIRECTION('center_axis',(0.,-1.,0.));
#5952=DIRECTION('ref_axis',(1.,0.,0.));
#5953=DIRECTION('',(0.,1.,0.));
#5954=DIRECTION('center_axis',(0.,1.,0.));
#5955=DIRECTION('ref_axis',(1.,0.,0.));
#5956=DIRECTION('center_axis',(0.,-1.,0.));
#5957=DIRECTION('ref_axis',(1.,0.,0.));
#5958=DIRECTION('',(-0.707106781186547,0.707106781186548,-8.65956056235493E-17));
#5959=DIRECTION('center_axis',(0.,-1.,0.));
#5960=DIRECTION('ref_axis',(0.,0.,-1.));
#5961=DIRECTION('center_axis',(0.,-1.,0.));
#5962=DIRECTION('ref_axis',(1.,0.,0.));
#5963=DIRECTION('center_axis',(0.,-1.,0.));
#5964=DIRECTION('ref_axis',(1.,0.,0.));
#5965=DIRECTION('',(0.,1.,0.));
#5966=DIRECTION('',(0.,0.,1.));
#5967=DIRECTION('',(1.,0.,0.));
#5968=DIRECTION('',(0.,0.,1.));
#5969=DIRECTION('',(1.,0.,0.));
#5970=DIRECTION('',(0.,0.,1.));
#5971=DIRECTION('',(1.,0.,0.));
#5972=DIRECTION('',(0.,0.,1.));
#5973=DIRECTION('',(1.,0.,0.));
#5974=DIRECTION('',(0.,0.,1.));
#5975=DIRECTION('',(1.,0.,0.));
#5976=DIRECTION('',(0.,0.,1.));
#5977=DIRECTION('',(1.,0.,0.));
#5978=DIRECTION('',(0.,0.,1.));
#5979=DIRECTION('',(1.,0.,0.));
#5980=DIRECTION('',(0.,0.,1.));
#5981=DIRECTION('',(1.,0.,0.));
#5982=DIRECTION('',(0.,0.,1.));
#5983=DIRECTION('',(1.,0.,0.));
#5984=DIRECTION('',(-1.,0.,2.22044604925031E-16));
#5985=DIRECTION('',(2.22044604925031E-16,0.,1.));
#5986=DIRECTION('',(0.,1.,2.22044604925031E-16));
#5987=DIRECTION('',(1.,0.,0.));
#5988=DIRECTION('',(0.,1.,2.22044604925031E-16));
#5989=DIRECTION('',(1.,0.,0.));
#5990=DIRECTION('',(0.,-1.,2.22044604925031E-16));
#5991=DIRECTION('',(1.,0.,0.));
#5992=DIRECTION('',(0.,-1.,2.22044604925031E-16));
#5993=DIRECTION('',(1.,0.,0.));
#5994=DIRECTION('',(0.,-1.,2.22044604925031E-16));
#5995=DIRECTION('',(1.,0.,0.));
#5996=DIRECTION('',(0.,-1.,2.22044604925031E-16));
#5997=DIRECTION('',(1.,0.,0.));
#5998=DIRECTION('',(0.,0.,1.));
#5999=DIRECTION('',(2.22044604925031E-16,-1.,0.));
#6000=DIRECTION('axis',(0.,0.,1.));
#6001=DIRECTION('refdir',(1.,0.,0.));
#6002=DIRECTION('axis',(0.,0.,1.));
#6003=DIRECTION('refdir',(1.,0.,0.));
#6004=DIRECTION('center_axis',(0.,1.,0.));
#6005=DIRECTION('ref_axis',(1.,0.,0.));
#6006=DIRECTION('center_axis',(0.,1.,0.));
#6007=DIRECTION('ref_axis',(1.,0.,0.));
#6008=DIRECTION('',(0.,1.,0.));
#6009=DIRECTION('center_axis',(0.,1.,0.));
#6010=DIRECTION('ref_axis',(1.,0.,0.));
#6011=DIRECTION('center_axis',(0.,1.,0.));
#6012=DIRECTION('ref_axis',(1.,0.,0.));
#6013=DIRECTION('center_axis',(0.,-1.,0.));
#6014=DIRECTION('ref_axis',(1.,0.,0.));
#6015=DIRECTION('center_axis',(0.,1.,0.));
#6016=DIRECTION('ref_axis',(1.,0.,0.));
#6017=DIRECTION('',(0.,1.,0.));
#6018=DIRECTION('center_axis',(0.,-1.,0.));
#6019=DIRECTION('ref_axis',(1.,-1.11022302462516E-15,0.));
#6020=DIRECTION('center_axis',(0.,1.,0.));
#6021=DIRECTION('ref_axis',(1.,0.,0.));
#6022=DIRECTION('center_axis',(0.,1.,0.));
#6023=DIRECTION('ref_axis',(1.,0.,0.));
#6024=DIRECTION('',(0.,-1.,0.));
#6025=DIRECTION('center_axis',(0.,1.,0.));
#6026=DIRECTION('ref_axis',(1.,0.,0.));
#6027=DIRECTION('center_axis',(0.,1.,0.));
#6028=DIRECTION('ref_axis',(1.,0.,0.));
#6029=DIRECTION('center_axis',(0.,0.,1.));
#6030=DIRECTION('ref_axis',(1.,0.,0.));
#6031=DIRECTION('center_axis',(0.,-1.,0.));
#6032=DIRECTION('ref_axis',(-1.,0.,0.));
#6033=DIRECTION('axis',(0.,0.,1.));
#6034=DIRECTION('refdir',(1.,0.,0.));
#6035=DIRECTION('center_axis',(0.,1.,0.));
#6036=DIRECTION('ref_axis',(1.,0.,0.));
#6037=DIRECTION('center_axis',(0.,-1.,0.));
#6038=DIRECTION('ref_axis',(1.,0.,0.));
#6039=DIRECTION('',(0.,-1.,0.));
#6040=DIRECTION('center_axis',(0.,-1.,0.));
#6041=DIRECTION('ref_axis',(1.,0.,0.));
#6042=DIRECTION('center_axis',(0.,1.,0.));
#6043=DIRECTION('ref_axis',(1.,0.,0.));
#6044=DIRECTION('center_axis',(0.,1.,0.));
#6045=DIRECTION('ref_axis',(1.,0.,0.));
#6046=DIRECTION('',(0.,-1.,0.));
#6047=DIRECTION('center_axis',(0.,1.,0.));
#6048=DIRECTION('ref_axis',(1.,0.,0.));
#6049=DIRECTION('center_axis',(0.,1.,0.));
#6050=DIRECTION('ref_axis',(1.,0.,0.));
#6051=DIRECTION('center_axis',(0.,1.,0.));
#6052=DIRECTION('ref_axis',(1.,0.,0.));
#6053=DIRECTION('axis',(0.,0.,1.));
#6054=DIRECTION('refdir',(1.,0.,0.));
#6055=DIRECTION('center_axis',(0.,1.,0.));
#6056=DIRECTION('ref_axis',(1.,0.,0.));
#6057=DIRECTION('center_axis',(0.,1.,0.));
#6058=DIRECTION('ref_axis',(1.,0.,0.));
#6059=DIRECTION('',(0.,1.,0.));
#6060=DIRECTION('center_axis',(0.,-1.,0.));
#6061=DIRECTION('ref_axis',(1.,0.,0.));
#6062=DIRECTION('center_axis',(0.,1.,0.));
#6063=DIRECTION('ref_axis',(1.,0.,0.));
#6064=DIRECTION('center_axis',(0.,1.,0.));
#6065=DIRECTION('ref_axis',(1.,0.,0.));
#6066=DIRECTION('center_axis',(0.,1.,0.));
#6067=DIRECTION('ref_axis',(1.,0.,0.));
#6068=DIRECTION('',(0.,-1.,0.));
#6069=DIRECTION('center_axis',(0.,-1.,0.));
#6070=DIRECTION('ref_axis',(1.,0.,0.));
#6071=DIRECTION('center_axis',(0.,1.,0.));
#6072=DIRECTION('ref_axis',(1.,0.,0.));
#6073=DIRECTION('center_axis',(0.,1.,0.));
#6074=DIRECTION('ref_axis',(1.,0.,0.));
#6075=DIRECTION('',(0.,-1.,0.));
#6076=DIRECTION('center_axis',(0.,1.,0.));
#6077=DIRECTION('ref_axis',(1.,0.,0.));
#6078=DIRECTION('center_axis',(0.,1.,0.));
#6079=DIRECTION('ref_axis',(1.,0.,0.));
#6080=DIRECTION('center_axis',(0.,1.,0.));
#6081=DIRECTION('ref_axis',(1.,0.,0.));
#6082=DIRECTION('axis',(0.,0.,1.));
#6083=DIRECTION('refdir',(1.,0.,0.));
#6084=DIRECTION('axis',(0.,0.,1.));
#6085=DIRECTION('refdir',(1.,0.,0.));
#6086=DIRECTION('center_axis',(0.,1.,0.));
#6087=DIRECTION('ref_axis',(1.,0.,0.));
#6088=DIRECTION('center_axis',(0.,1.,0.));
#6089=DIRECTION('ref_axis',(1.,0.,0.));
#6090=DIRECTION('',(0.,1.,0.));
#6091=DIRECTION('center_axis',(0.,1.,0.));
#6092=DIRECTION('ref_axis',(1.,0.,0.));
#6093=DIRECTION('center_axis',(0.,1.,0.));
#6094=DIRECTION('ref_axis',(1.,0.,0.));
#6095=DIRECTION('center_axis',(0.,-1.,0.));
#6096=DIRECTION('ref_axis',(1.,0.,0.));
#6097=DIRECTION('center_axis',(0.,1.,0.));
#6098=DIRECTION('ref_axis',(1.,0.,0.));
#6099=DIRECTION('',(0.,1.,0.));
#6100=DIRECTION('center_axis',(0.,-1.,0.));
#6101=DIRECTION('ref_axis',(1.,-1.11022302462516E-15,0.));
#6102=DIRECTION('center_axis',(0.,1.,0.));
#6103=DIRECTION('ref_axis',(1.,0.,0.));
#6104=DIRECTION('center_axis',(0.,1.,0.));
#6105=DIRECTION('ref_axis',(1.,0.,0.));
#6106=DIRECTION('',(0.,-1.,0.));
#6107=DIRECTION('center_axis',(0.,1.,0.));
#6108=DIRECTION('ref_axis',(1.,0.,0.));
#6109=DIRECTION('center_axis',(0.,1.,0.));
#6110=DIRECTION('ref_axis',(1.,0.,0.));
#6111=DIRECTION('center_axis',(6.12323399573677E-17,0.,1.));
#6112=DIRECTION('ref_axis',(1.,0.,0.));
#6113=DIRECTION('center_axis',(0.,-1.,0.));
#6114=DIRECTION('ref_axis',(-1.,0.,0.));
#6115=DIRECTION('axis',(0.,0.,1.));
#6116=DIRECTION('refdir',(1.,0.,0.));
#6117=DIRECTION('center_axis',(0.,1.,0.));
#6118=DIRECTION('ref_axis',(1.,0.,0.));
#6119=DIRECTION('center_axis',(0.,-1.,0.));
#6120=DIRECTION('ref_axis',(1.,0.,0.));
#6121=DIRECTION('',(0.,-1.,0.));
#6122=DIRECTION('center_axis',(0.,-1.,0.));
#6123=DIRECTION('ref_axis',(1.,0.,0.));
#6124=DIRECTION('center_axis',(0.,1.,0.));
#6125=DIRECTION('ref_axis',(1.,0.,0.));
#6126=DIRECTION('center_axis',(0.,1.,0.));
#6127=DIRECTION('ref_axis',(1.,0.,0.));
#6128=DIRECTION('',(0.,-1.,0.));
#6129=DIRECTION('center_axis',(0.,1.,0.));
#6130=DIRECTION('ref_axis',(1.,0.,0.));
#6131=DIRECTION('center_axis',(0.,1.,0.));
#6132=DIRECTION('ref_axis',(1.,0.,0.));
#6133=DIRECTION('center_axis',(0.,1.,0.));
#6134=DIRECTION('ref_axis',(1.,0.,0.));
#6135=DIRECTION('axis',(0.,0.,1.));
#6136=DIRECTION('refdir',(1.,0.,0.));
#6137=DIRECTION('center_axis',(0.,1.,0.));
#6138=DIRECTION('ref_axis',(1.,0.,0.));
#6139=DIRECTION('center_axis',(0.,1.,0.));
#6140=DIRECTION('ref_axis',(1.,0.,0.));
#6141=DIRECTION('',(0.,1.,0.));
#6142=DIRECTION('center_axis',(0.,-1.,0.));
#6143=DIRECTION('ref_axis',(1.,0.,0.));
#6144=DIRECTION('center_axis',(0.,1.,0.));
#6145=DIRECTION('ref_axis',(1.,0.,0.));
#6146=DIRECTION('center_axis',(0.,1.,0.));
#6147=DIRECTION('ref_axis',(1.,0.,0.));
#6148=DIRECTION('center_axis',(0.,1.,0.));
#6149=DIRECTION('ref_axis',(1.,0.,0.));
#6150=DIRECTION('',(0.,-1.,0.));
#6151=DIRECTION('center_axis',(0.,-1.,0.));
#6152=DIRECTION('ref_axis',(1.,0.,0.));
#6153=DIRECTION('center_axis',(0.,1.,0.));
#6154=DIRECTION('ref_axis',(1.,0.,0.));
#6155=DIRECTION('center_axis',(0.,1.,0.));
#6156=DIRECTION('ref_axis',(1.,0.,0.));
#6157=DIRECTION('',(0.,-1.,0.));
#6158=DIRECTION('center_axis',(0.,1.,0.));
#6159=DIRECTION('ref_axis',(1.,0.,0.));
#6160=DIRECTION('center_axis',(0.,1.,0.));
#6161=DIRECTION('ref_axis',(1.,0.,0.));
#6162=DIRECTION('center_axis',(0.,1.,0.));
#6163=DIRECTION('ref_axis',(1.,0.,0.));
#6164=DIRECTION('axis',(0.,0.,1.));
#6165=DIRECTION('refdir',(1.,0.,0.));
#6166=DIRECTION('axis',(0.,0.,1.));
#6167=DIRECTION('refdir',(1.,0.,0.));
#6168=DIRECTION('center_axis',(0.,1.,0.));
#6169=DIRECTION('ref_axis',(1.,0.,0.));
#6170=DIRECTION('center_axis',(0.,1.,0.));
#6171=DIRECTION('ref_axis',(1.,0.,0.));
#6172=DIRECTION('',(0.,1.,0.));
#6173=DIRECTION('center_axis',(0.,1.,0.));
#6174=DIRECTION('ref_axis',(1.,0.,0.));
#6175=DIRECTION('center_axis',(0.,1.,0.));
#6176=DIRECTION('ref_axis',(1.,0.,0.));
#6177=DIRECTION('center_axis',(0.,-1.,0.));
#6178=DIRECTION('ref_axis',(1.,0.,0.));
#6179=DIRECTION('center_axis',(0.,1.,0.));
#6180=DIRECTION('ref_axis',(1.,0.,0.));
#6181=DIRECTION('',(0.,1.,0.));
#6182=DIRECTION('center_axis',(0.,-1.,0.));
#6183=DIRECTION('ref_axis',(1.,-1.11022302462516E-15,0.));
#6184=DIRECTION('center_axis',(0.,1.,0.));
#6185=DIRECTION('ref_axis',(1.,0.,0.));
#6186=DIRECTION('center_axis',(0.,1.,0.));
#6187=DIRECTION('ref_axis',(1.,0.,0.));
#6188=DIRECTION('',(0.,-1.,0.));
#6189=DIRECTION('center_axis',(0.,1.,0.));
#6190=DIRECTION('ref_axis',(1.,0.,0.));
#6191=DIRECTION('center_axis',(0.,1.,0.));
#6192=DIRECTION('ref_axis',(1.,0.,0.));
#6193=DIRECTION('center_axis',(0.,0.,1.));
#6194=DIRECTION('ref_axis',(1.,0.,0.));
#6195=DIRECTION('center_axis',(0.,-1.,0.));
#6196=DIRECTION('ref_axis',(-1.,0.,0.));
#6197=DIRECTION('axis',(0.,0.,1.));
#6198=DIRECTION('refdir',(1.,0.,0.));
#6199=DIRECTION('center_axis',(0.,1.,0.));
#6200=DIRECTION('ref_axis',(1.,0.,0.));
#6201=DIRECTION('center_axis',(0.,-1.,0.));
#6202=DIRECTION('ref_axis',(1.,0.,0.));
#6203=DIRECTION('',(0.,-1.,0.));
#6204=DIRECTION('center_axis',(0.,-1.,0.));
#6205=DIRECTION('ref_axis',(1.,0.,0.));
#6206=DIRECTION('center_axis',(0.,1.,0.));
#6207=DIRECTION('ref_axis',(1.,0.,0.));
#6208=DIRECTION('center_axis',(0.,1.,0.));
#6209=DIRECTION('ref_axis',(1.,0.,0.));
#6210=DIRECTION('',(0.,-1.,0.));
#6211=DIRECTION('center_axis',(0.,1.,0.));
#6212=DIRECTION('ref_axis',(1.,0.,0.));
#6213=DIRECTION('center_axis',(0.,1.,0.));
#6214=DIRECTION('ref_axis',(1.,0.,0.));
#6215=DIRECTION('center_axis',(0.,1.,0.));
#6216=DIRECTION('ref_axis',(1.,0.,0.));
#6217=DIRECTION('axis',(0.,0.,1.));
#6218=DIRECTION('refdir',(1.,0.,0.));
#6219=DIRECTION('center_axis',(0.,1.,0.));
#6220=DIRECTION('ref_axis',(1.,0.,0.));
#6221=DIRECTION('center_axis',(0.,1.,0.));
#6222=DIRECTION('ref_axis',(1.,0.,0.));
#6223=DIRECTION('',(0.,1.,0.));
#6224=DIRECTION('center_axis',(0.,-1.,0.));
#6225=DIRECTION('ref_axis',(1.,0.,0.));
#6226=DIRECTION('center_axis',(0.,1.,0.));
#6227=DIRECTION('ref_axis',(1.,0.,0.));
#6228=DIRECTION('center_axis',(0.,1.,0.));
#6229=DIRECTION('ref_axis',(1.,0.,0.));
#6230=DIRECTION('center_axis',(0.,1.,0.));
#6231=DIRECTION('ref_axis',(1.,0.,0.));
#6232=DIRECTION('',(0.,-1.,0.));
#6233=DIRECTION('center_axis',(0.,-1.,0.));
#6234=DIRECTION('ref_axis',(1.,0.,0.));
#6235=DIRECTION('center_axis',(0.,1.,0.));
#6236=DIRECTION('ref_axis',(1.,0.,0.));
#6237=DIRECTION('center_axis',(0.,1.,0.));
#6238=DIRECTION('ref_axis',(1.,0.,0.));
#6239=DIRECTION('',(0.,-1.,0.));
#6240=DIRECTION('center_axis',(0.,1.,0.));
#6241=DIRECTION('ref_axis',(1.,0.,0.));
#6242=DIRECTION('center_axis',(0.,1.,0.));
#6243=DIRECTION('ref_axis',(1.,0.,0.));
#6244=DIRECTION('center_axis',(0.,1.,0.));
#6245=DIRECTION('ref_axis',(1.,0.,0.));
#6246=DIRECTION('axis',(0.,0.,1.));
#6247=DIRECTION('refdir',(1.,0.,0.));
#6248=DIRECTION('axis',(0.,0.,1.));
#6249=DIRECTION('refdir',(1.,0.,0.));
#6250=DIRECTION('center_axis',(0.,1.,0.));
#6251=DIRECTION('ref_axis',(1.,0.,0.));
#6252=DIRECTION('center_axis',(0.,1.,0.));
#6253=DIRECTION('ref_axis',(1.,0.,0.));
#6254=DIRECTION('',(0.,1.,0.));
#6255=DIRECTION('center_axis',(0.,-1.,0.));
#6256=DIRECTION('ref_axis',(1.,0.,0.));
#6257=DIRECTION('center_axis',(0.,1.,0.));
#6258=DIRECTION('ref_axis',(1.,0.,0.));
#6259=DIRECTION('center_axis',(0.,1.,0.));
#6260=DIRECTION('ref_axis',(1.,0.,0.));
#6261=DIRECTION('center_axis',(0.,1.,0.));
#6262=DIRECTION('ref_axis',(1.,0.,0.));
#6263=DIRECTION('',(0.5,0.,-0.866025403784439));
#6264=DIRECTION('',(-0.5,0.,-0.866025403784439));
#6265=DIRECTION('',(-1.,0.,-1.60246890531964E-16));
#6266=DIRECTION('',(-0.5,0.,0.866025403784439));
#6267=DIRECTION('',(0.5,0.,0.866025403784439));
#6268=DIRECTION('',(1.,0.,1.60246890531964E-16));
#6269=DIRECTION('center_axis',(0.,-1.,0.));
#6270=DIRECTION('ref_axis',(1.,0.,0.));
#6271=DIRECTION('center_axis',(0.,1.,0.));
#6272=DIRECTION('ref_axis',(1.,0.,0.));
#6273=DIRECTION('',(0.5,0.,-0.866025403784439));
#6274=DIRECTION('',(1.,0.,1.60246890531964E-16));
#6275=DIRECTION('',(0.5,0.,0.866025403784439));
#6276=DIRECTION('',(-0.5,0.,0.866025403784439));
#6277=DIRECTION('',(-1.,0.,-1.60246890531964E-16));
#6278=DIRECTION('',(-0.5,0.,-0.866025403784439));
#6279=DIRECTION('center_axis',(0.,-1.,0.));
#6280=DIRECTION('ref_axis',(1.,0.,0.));
#6281=DIRECTION('center_axis',(-1.60246890531964E-16,0.,1.));
#6282=DIRECTION('ref_axis',(1.,0.,1.60246890531964E-16));
#6283=DIRECTION('',(0.,1.,0.));
#6284=DIRECTION('',(0.,1.,0.));
#6285=DIRECTION('center_axis',(-0.866025403784439,0.,0.5));
#6286=DIRECTION('ref_axis',(0.5,0.,0.866025403784439));
#6287=DIRECTION('',(0.,1.,0.));
#6288=DIRECTION('center_axis',(-0.866025403784439,0.,-0.5));
#6289=DIRECTION('ref_axis',(-0.5,0.,0.866025403784439));
#6290=DIRECTION('',(0.,1.,0.));
#6291=DIRECTION('center_axis',(1.60246890531964E-16,0.,-1.));
#6292=DIRECTION('ref_axis',(-1.,0.,-1.60246890531964E-16));
#6293=DIRECTION('',(0.,1.,0.));
#6294=DIRECTION('center_axis',(0.866025403784439,0.,-0.5));
#6295=DIRECTION('ref_axis',(-0.5,0.,-0.866025403784439));
#6296=DIRECTION('',(0.,1.,0.));
#6297=DIRECTION('center_axis',(0.866025403784439,0.,0.5));
#6298=DIRECTION('ref_axis',(0.5,0.,-0.866025403784439));
#6299=DIRECTION('center_axis',(0.,1.,0.));
#6300=DIRECTION('ref_axis',(0.,0.,1.));
#6301=DIRECTION('center_axis',(0.,-1.,0.));
#6302=DIRECTION('ref_axis',(1.,0.,0.));
#6303=DIRECTION('center_axis',(0.,-1.,0.));
#6304=DIRECTION('ref_axis',(1.,0.,0.));
#6305=DIRECTION('',(0.,1.,0.));
#6306=DIRECTION('center_axis',(0.,-1.,0.));
#6307=DIRECTION('ref_axis',(1.,0.,0.));
#6308=DIRECTION('center_axis',(0.,1.,0.));
#6309=DIRECTION('ref_axis',(0.,0.,1.));
#6310=DIRECTION('center_axis',(0.,-1.,0.));
#6311=DIRECTION('ref_axis',(1.,0.,0.));
#6312=DIRECTION('center_axis',(0.,-1.,0.));
#6313=DIRECTION('ref_axis',(1.,0.,0.));
#6314=DIRECTION('',(0.,1.,0.));
#6315=DIRECTION('center_axis',(0.,-1.,0.));
#6316=DIRECTION('ref_axis',(1.,0.,0.));
#6317=DIRECTION('center_axis',(0.,-1.,0.));
#6318=DIRECTION('ref_axis',(1.,0.,0.));
#6319=DIRECTION('',(0.,1.,0.));
#6320=DIRECTION('center_axis',(0.,-1.,0.));
#6321=DIRECTION('ref_axis',(0.,0.,-1.));
#6322=DIRECTION('center_axis',(0.,-1.,0.));
#6323=DIRECTION('ref_axis',(1.,0.,0.));
#6324=DIRECTION('center_axis',(0.,-1.,0.));
#6325=DIRECTION('ref_axis',(1.,0.,0.));
#6326=DIRECTION('',(0.,1.,0.));
#6327=DIRECTION('axis',(0.,0.,1.));
#6328=DIRECTION('refdir',(1.,0.,0.));
#6329=DIRECTION('center_axis',(0.,1.,0.));
#6330=DIRECTION('ref_axis',(0.,0.,1.));
#6331=DIRECTION('center_axis',(0.,-1.,0.));
#6332=DIRECTION('ref_axis',(1.,0.,0.));
#6333=DIRECTION('center_axis',(0.,-1.,0.));
#6334=DIRECTION('ref_axis',(1.,0.,0.));
#6335=DIRECTION('center_axis',(0.,-1.,0.));
#6336=DIRECTION('ref_axis',(1.,0.,0.));
#6337=DIRECTION('center_axis',(0.,-1.,0.));
#6338=DIRECTION('ref_axis',(1.,0.,0.));
#6339=DIRECTION('',(0.,1.,0.));
#6340=DIRECTION('center_axis',(0.,-1.,0.));
#6341=DIRECTION('ref_axis',(0.,0.,-1.));
#6342=DIRECTION('center_axis',(0.,-1.,0.));
#6343=DIRECTION('ref_axis',(1.,0.,0.));
#6344=DIRECTION('center_axis',(0.,-1.,0.));
#6345=DIRECTION('ref_axis',(1.,0.,0.));
#6346=DIRECTION('center_axis',(0.,-1.,0.));
#6347=DIRECTION('ref_axis',(1.,0.,0.));
#6348=DIRECTION('',(0.,1.,0.));
#6349=DIRECTION('center_axis',(0.,-1.,0.));
#6350=DIRECTION('ref_axis',(0.,0.,-1.));
#6351=DIRECTION('center_axis',(0.,-1.,0.));
#6352=DIRECTION('ref_axis',(1.,0.,0.));
#6353=DIRECTION('center_axis',(0.,-1.,0.));
#6354=DIRECTION('ref_axis',(1.,0.,0.));
#6355=DIRECTION('',(0.,1.,0.));
#6356=DIRECTION('',(0.,0.,1.));
#6357=DIRECTION('',(1.,0.,0.));
#6358=DIRECTION('',(0.,0.,1.));
#6359=DIRECTION('',(1.,0.,0.));
#6360=DIRECTION('',(0.,0.,1.));
#6361=DIRECTION('',(1.,0.,0.));
#6362=DIRECTION('',(0.,0.,1.));
#6363=DIRECTION('',(1.,0.,0.));
#6364=DIRECTION('',(0.,0.,1.));
#6365=DIRECTION('',(1.,0.,0.));
#6366=DIRECTION('',(0.,0.,1.));
#6367=DIRECTION('',(-1.,1.22464679914735E-16,0.));
#6368=DIRECTION('',(0.,0.,1.));
#6369=DIRECTION('',(1.,0.,0.));
#6370=DIRECTION('',(0.,0.,1.));
#6371=DIRECTION('',(1.,0.,0.));
#6372=DIRECTION('',(0.,0.,1.));
#6373=DIRECTION('',(1.,0.,0.));
#6374=DIRECTION('',(0.,0.,1.));
#6375=DIRECTION('',(-1.,1.22464679914735E-16,0.));
#6376=DIRECTION('',(0.,0.,1.));
#6377=DIRECTION('',(1.,0.,0.));
#6378=DIRECTION('',(0.,0.,1.));
#6379=DIRECTION('',(1.,0.,0.));
#6380=DIRECTION('',(0.,0.,1.));
#6381=DIRECTION('',(1.,0.,0.));
#6382=DIRECTION('',(0.,0.,1.));
#6383=DIRECTION('',(-1.,1.22464679914735E-16,0.));
#6384=DIRECTION('',(0.,0.,1.));
#6385=DIRECTION('',(1.,0.,0.));
#6386=DIRECTION('',(0.,0.,1.));
#6387=DIRECTION('',(1.,0.,0.));
#6388=DIRECTION('',(0.,0.,1.));
#6389=DIRECTION('',(1.,0.,0.));
#6390=DIRECTION('',(0.,0.,1.));
#6391=DIRECTION('',(1.,0.,0.));
#6392=CARTESIAN_POINT('',(0.,0.,0.));
#6393=CARTESIAN_POINT('',(0.,0.,0.));
#6394=CARTESIAN_POINT('',(0.,0.,0.));
#6395=CARTESIAN_POINT('Origin',(0.,3.,-0.1));
#6396=CARTESIAN_POINT('',(-0.275,3.,0.));
#6397=CARTESIAN_POINT('Origin',(0.,3.,0.));
#6398=CARTESIAN_POINT('',(-0.275,3.,0.8));
#6399=CARTESIAN_POINT('',(-0.275,3.,-0.1));
#6400=CARTESIAN_POINT('Origin',(0.,3.,0.8));
#6401=CARTESIAN_POINT('Origin',(6.,6.,0.));
#6402=CARTESIAN_POINT('',(6.,6.,0.));
#6403=CARTESIAN_POINT('',(-6.,6.,0.));
#6404=CARTESIAN_POINT('',(6.,6.,0.));
#6405=CARTESIAN_POINT('',(-6.,6.,0.8));
#6406=CARTESIAN_POINT('',(-6.,6.,0.));
#6407=CARTESIAN_POINT('',(6.,6.,0.8));
#6408=CARTESIAN_POINT('',(6.,6.,0.8));
#6409=CARTESIAN_POINT('',(6.,6.,0.));
#6410=CARTESIAN_POINT('Origin',(6.,-4.,0.));
#6411=CARTESIAN_POINT('',(6.,-4.,0.));
#6412=CARTESIAN_POINT('',(6.,-4.,0.));
#6413=CARTESIAN_POINT('',(6.,-4.,0.8));
#6414=CARTESIAN_POINT('',(6.,-4.,0.8));
#6415=CARTESIAN_POINT('',(6.,-4.,0.));
#6416=CARTESIAN_POINT('Origin',(-6.,-4.,0.));
#6417=CARTESIAN_POINT('',(-6.,-4.,0.));
#6418=CARTESIAN_POINT('',(-6.,-4.,0.));
#6419=CARTESIAN_POINT('',(-6.,-4.,0.8));
#6420=CARTESIAN_POINT('',(-6.,-4.,0.8));
#6421=CARTESIAN_POINT('',(-6.,-4.,0.));
#6422=CARTESIAN_POINT('Origin',(-6.,6.,0.));
#6423=CARTESIAN_POINT('',(-6.,6.,0.));
#6424=CARTESIAN_POINT('',(-6.,6.,0.8));
#6425=CARTESIAN_POINT('Origin',(0.,1.,0.8));
#6426=CARTESIAN_POINT('Origin',(0.,1.,0.));
#6427=CARTESIAN_POINT('',(0.,0.,0.));
#6428=CARTESIAN_POINT('Origin',(-4.,6.,-0.8));
#6429=CARTESIAN_POINT('',(-4.,6.,-0.8));
#6430=CARTESIAN_POINT('',(-6.,6.,-0.8));
#6431=CARTESIAN_POINT('',(-4.,6.,-0.8));
#6432=CARTESIAN_POINT('',(-6.,6.,0.));
#6433=CARTESIAN_POINT('',(-6.,6.,-0.8));
#6434=CARTESIAN_POINT('',(-4.,6.,0.));
#6435=CARTESIAN_POINT('',(-4.,6.,0.));
#6436=CARTESIAN_POINT('',(-4.,6.,-0.8));
#6437=CARTESIAN_POINT('Origin',(-4.,-4.,-0.8));
#6438=CARTESIAN_POINT('',(-4.,-4.,-0.8));
#6439=CARTESIAN_POINT('',(-4.,-4.,-0.8));
#6440=CARTESIAN_POINT('',(-4.,-4.,0.));
#6441=CARTESIAN_POINT('',(-4.,-4.,0.));
#6442=CARTESIAN_POINT('',(-4.,-4.,-0.8));
#6443=CARTESIAN_POINT('Origin',(-6.,-4.,-0.8));
#6444=CARTESIAN_POINT('',(-6.,-4.,-0.8));
#6445=CARTESIAN_POINT('',(-6.,-4.,-0.8));
#6446=CARTESIAN_POINT('',(-6.,-4.,0.));
#6447=CARTESIAN_POINT('',(-6.,-4.,0.));
#6448=CARTESIAN_POINT('',(-6.,-4.,-0.8));
#6449=CARTESIAN_POINT('Origin',(-6.,6.,-0.8));
#6450=CARTESIAN_POINT('',(-6.,6.,-0.8));
#6451=CARTESIAN_POINT('',(-6.,6.,0.));
#6452=CARTESIAN_POINT('Origin',(-5.,1.,0.));
#6453=CARTESIAN_POINT('Origin',(-5.,1.,-0.8));
#6454=CARTESIAN_POINT('',(0.,0.,0.));
#6455=CARTESIAN_POINT('Origin',(6.,6.,-0.8));
#6456=CARTESIAN_POINT('',(6.,6.,-0.8));
#6457=CARTESIAN_POINT('',(4.,6.,-0.8));
#6458=CARTESIAN_POINT('',(6.,6.,-0.8));
#6459=CARTESIAN_POINT('',(4.,6.,0.));
#6460=CARTESIAN_POINT('',(4.,6.,-0.8));
#6461=CARTESIAN_POINT('',(6.,6.,0.));
#6462=CARTESIAN_POINT('',(6.,6.,0.));
#6463=CARTESIAN_POINT('',(6.,6.,-0.8));
#6464=CARTESIAN_POINT('Origin',(6.,-4.,-0.8));
#6465=CARTESIAN_POINT('',(6.,-4.,-0.8));
#6466=CARTESIAN_POINT('',(6.,-4.,-0.8));
#6467=CARTESIAN_POINT('',(6.,-4.,0.));
#6468=CARTESIAN_POINT('',(6.,-4.,0.));
#6469=CARTESIAN_POINT('',(6.,-4.,-0.8));
#6470=CARTESIAN_POINT('Origin',(4.,-4.,-0.8));
#6471=CARTESIAN_POINT('',(4.,-4.,-0.8));
#6472=CARTESIAN_POINT('',(4.,-4.,-0.8));
#6473=CARTESIAN_POINT('',(4.,-4.,0.));
#6474=CARTESIAN_POINT('',(4.,-4.,0.));
#6475=CARTESIAN_POINT('',(4.,-4.,-0.8));
#6476=CARTESIAN_POINT('Origin',(4.,6.,-0.8));
#6477=CARTESIAN_POINT('',(4.,6.,-0.8));
#6478=CARTESIAN_POINT('',(4.,6.,0.));
#6479=CARTESIAN_POINT('Origin',(5.,1.,0.));
#6480=CARTESIAN_POINT('Origin',(5.,1.,-0.8));
#6481=CARTESIAN_POINT('',(0.,0.,0.));
#6482=CARTESIAN_POINT('Origin',(-4.3,1.,20.7));
#6483=CARTESIAN_POINT('',(-4.465,1.,20.8));
#6484=CARTESIAN_POINT('Origin',(-4.3,1.,20.8));
#6485=CARTESIAN_POINT('',(-4.465,1.,21.5));
#6486=CARTESIAN_POINT('',(-4.465,1.,20.7));
#6487=CARTESIAN_POINT('Origin',(-4.3,1.,21.5));
#6488=CARTESIAN_POINT('Origin',(4.3,1.,20.7));
#6489=CARTESIAN_POINT('',(4.135,1.,20.8));
#6490=CARTESIAN_POINT('Origin',(4.3,1.,20.8));
#6491=CARTESIAN_POINT('',(4.135,1.,21.5));
#6492=CARTESIAN_POINT('',(4.135,1.,20.7));
#6493=CARTESIAN_POINT('Origin',(4.3,1.,21.5));
#6494=CARTESIAN_POINT('Origin',(0.,3.,20.7));
#6495=CARTESIAN_POINT('',(-0.275,3.,20.8));
#6496=CARTESIAN_POINT('Origin',(0.,3.,20.8));
#6497=CARTESIAN_POINT('',(-0.275,3.,21.5));
#6498=CARTESIAN_POINT('',(-0.275,3.,20.7));
#6499=CARTESIAN_POINT('Origin',(0.,3.,21.5));
#6500=CARTESIAN_POINT('Origin',(5.5,4.,20.8));
#6501=CARTESIAN_POINT('',(5.5,4.,20.8));
#6502=CARTESIAN_POINT('',(-5.5,4.,20.8));
#6503=CARTESIAN_POINT('',(5.5,4.,20.8));
#6504=CARTESIAN_POINT('',(-5.5,4.,21.5));
#6505=CARTESIAN_POINT('',(-5.5,4.,20.8));
#6506=CARTESIAN_POINT('',(5.5,4.,21.5));
#6507=CARTESIAN_POINT('',(5.5,4.,21.5));
#6508=CARTESIAN_POINT('',(5.5,4.,20.8));
#6509=CARTESIAN_POINT('Origin',(5.5,-1.5,20.8));
#6510=CARTESIAN_POINT('',(5.5,-1.5,20.8));
#6511=CARTESIAN_POINT('',(5.5,-1.5,20.8));
#6512=CARTESIAN_POINT('',(5.5,-1.5,21.5));
#6513=CARTESIAN_POINT('',(5.5,-1.5,21.5));
#6514=CARTESIAN_POINT('',(5.5,-1.5,20.8));
#6515=CARTESIAN_POINT('Origin',(-5.5,-1.5,20.8));
#6516=CARTESIAN_POINT('',(-5.5,-1.5,20.8));
#6517=CARTESIAN_POINT('',(-5.5,-1.5,20.8));
#6518=CARTESIAN_POINT('',(-5.5,-1.5,21.5));
#6519=CARTESIAN_POINT('',(-5.5,-1.5,21.5));
#6520=CARTESIAN_POINT('',(-5.5,-1.5,20.8));
#6521=CARTESIAN_POINT('Origin',(-5.5,4.,20.8));
#6522=CARTESIAN_POINT('',(-5.5,4.,20.8));
#6523=CARTESIAN_POINT('',(-5.5,4.,21.5));
#6524=CARTESIAN_POINT('Origin',(0.,1.25,21.5));
#6525=CARTESIAN_POINT('Origin',(0.,1.25,20.8));
#6526=CARTESIAN_POINT('',(0.,0.,0.));
#6527=CARTESIAN_POINT('Origin',(3.,0.1,23.));
#6528=CARTESIAN_POINT('',(3.28284271247462,0.1,23.2828427124746));
#6529=CARTESIAN_POINT('',(2.71715728752538,0.1,23.2828427124746));
#6530=CARTESIAN_POINT('',(-5.1,0.1,23.2828427124746));
#6531=CARTESIAN_POINT('Origin',(3.,0.1,23.));
#6532=CARTESIAN_POINT('Origin',(3.,-2.1,23.));
#6533=CARTESIAN_POINT('',(2.6,-1.,23.));
#6534=CARTESIAN_POINT('Origin',(3.,-1.,23.));
#6535=CARTESIAN_POINT('',(2.6,-0.300000000000001,23.));
#6536=CARTESIAN_POINT('',(2.6,-2.1,23.));
#6537=CARTESIAN_POINT('',(2.73542486889354,-2.01044254631871E-17,23.3));
#6538=CARTESIAN_POINT('Ctrl Pts',(2.73542486889354,7.63278329429795E-17,
23.3));
#6539=CARTESIAN_POINT('Ctrl Pts',(2.73542486889354,-0.0201446772150695,
23.3));
#6540=CARTESIAN_POINT('Ctrl Pts',(2.73305334341681,-0.0403635841555968,
23.2979507721165));
#6541=CARTESIAN_POINT('Ctrl Pts',(2.7243365294397,-0.0797436599168342,23.2899048648568));
#6542=CARTESIAN_POINT('Ctrl Pts',(2.71802972961529,-0.0989142979472494,
23.2839128832536));
#6543=CARTESIAN_POINT('Ctrl Pts',(2.69593643019745,-0.153499080170581,23.2607687447172));
#6544=CARTESIAN_POINT('Ctrl Pts',(2.67718134717306,-0.186078125959879,23.2381859427521));
#6545=CARTESIAN_POINT('Ctrl Pts',(2.64492844776862,-0.237637949853887,23.186626118858));
#6546=CARTESIAN_POINT('Ctrl Pts',(2.62882756515854,-0.260548600882861,23.1539823555528));
#6547=CARTESIAN_POINT('Ctrl Pts',(2.60628603952013,-0.291765800294272,23.0804292530598));
#6548=CARTESIAN_POINT('Ctrl Pts',(2.6,-0.300000000000001,23.0394419468257));
#6549=CARTESIAN_POINT('Ctrl Pts',(2.6,-0.300000000000001,23.));
#6550=CARTESIAN_POINT('Ctrl Pts',(2.71715728752538,0.0999999999999983,23.2828427124746));
#6551=CARTESIAN_POINT('Ctrl Pts',(2.72174110582733,0.0870350039798468,23.2874265307766));
#6552=CARTESIAN_POINT('Ctrl Pts',(2.72568156083597,0.0736671922504066,23.2911463732685));
#6553=CARTESIAN_POINT('Ctrl Pts',(2.73305334341681,0.0403635841555971,23.2979507721165));
#6554=CARTESIAN_POINT('Ctrl Pts',(2.73542486889354,0.0201446772150696,23.3));
#6555=CARTESIAN_POINT('Ctrl Pts',(2.73542486889354,-6.93889390390723E-18,
23.3));
#6556=CARTESIAN_POINT('',(3.26457513110646,-1.40328932972683E-17,23.3));
#6557=CARTESIAN_POINT('Ctrl Pts',(3.26457513110646,-5.20417042793042E-18,
23.3));
#6558=CARTESIAN_POINT('Ctrl Pts',(3.26457513110646,0.0201446772150696,23.3));
#6559=CARTESIAN_POINT('Ctrl Pts',(3.26694665658319,0.0403635841555968,23.2979507721165));
#6560=CARTESIAN_POINT('Ctrl Pts',(3.27431843921387,0.0736671924755579,23.2911463732225));
#6561=CARTESIAN_POINT('Ctrl Pts',(3.27825889407742,0.0870350037104556,23.2874265308718));
#6562=CARTESIAN_POINT('Ctrl Pts',(3.28284271247462,0.0999999999999993,23.2828427124746));
#6563=CARTESIAN_POINT('',(3.28284271247462,0.1,22.7171572875254));
#6564=CARTESIAN_POINT('Ctrl Pts',(3.28284271247462,0.1,22.7171572875254));
#6565=CARTESIAN_POINT('Ctrl Pts',(3.27825889417267,0.0870350039798476,22.7125734692234));
#6566=CARTESIAN_POINT('Ctrl Pts',(3.27431843916403,0.0736671922504055,22.7088536267315));
#6567=CARTESIAN_POINT('Ctrl Pts',(3.26694665658319,0.0403635841555954,22.7020492278835));
#6568=CARTESIAN_POINT('Ctrl Pts',(3.26457513110646,0.0201446772150696,22.7));
#6569=CARTESIAN_POINT('Ctrl Pts',(3.26457513110646,0.,22.7));
#6570=CARTESIAN_POINT('Ctrl Pts',(3.26457513110646,-0.0201446772150696,
22.7));
#6571=CARTESIAN_POINT('Ctrl Pts',(3.26694665658319,-0.0403635841555971,
22.7020492278835));
#6572=CARTESIAN_POINT('Ctrl Pts',(3.2756634705603,-0.0797436599168345,22.7100951351432));
#6573=CARTESIAN_POINT('Ctrl Pts',(3.28197027038471,-0.0989142979472495,
22.7160871167464));
#6574=CARTESIAN_POINT('Ctrl Pts',(3.30406356980255,-0.153499080170581,22.7392312552828));
#6575=CARTESIAN_POINT('Ctrl Pts',(3.32281865282694,-0.186078125959879,22.7618140572479));
#6576=CARTESIAN_POINT('Ctrl Pts',(3.35507155223138,-0.237637949853888,22.813373881142));
#6577=CARTESIAN_POINT('Ctrl Pts',(3.37117243484146,-0.260548600882862,22.8460176444472));
#6578=CARTESIAN_POINT('Ctrl Pts',(3.39371396047987,-0.291765800294272,22.9195707469402));
#6579=CARTESIAN_POINT('Ctrl Pts',(3.4,-0.300000000000001,22.9605580531743));
#6580=CARTESIAN_POINT('Ctrl Pts',(3.4,-0.300000000000001,23.0394419468257));
#6581=CARTESIAN_POINT('Ctrl Pts',(3.39371396047987,-0.291765800294272,23.0804292530598));
#6582=CARTESIAN_POINT('Ctrl Pts',(3.37117243484146,-0.260548600882861,23.1539823555528));
#6583=CARTESIAN_POINT('Ctrl Pts',(3.35507155223138,-0.237637949853888,23.186626118858));
#6584=CARTESIAN_POINT('Ctrl Pts',(3.32281865282694,-0.186078125959879,23.2381859427521));
#6585=CARTESIAN_POINT('Ctrl Pts',(3.30406356980255,-0.153499080170581,23.2607687447172));
#6586=CARTESIAN_POINT('Ctrl Pts',(3.28197027038471,-0.0989142979472494,
23.2839128832536));
#6587=CARTESIAN_POINT('Ctrl Pts',(3.2756634705603,-0.0797436599168341,23.2899048648568));
#6588=CARTESIAN_POINT('Ctrl Pts',(3.26694665658319,-0.0403635841555968,
23.2979507721165));
#6589=CARTESIAN_POINT('Ctrl Pts',(3.26457513110646,-0.0201446772150696,
23.3));
#6590=CARTESIAN_POINT('Ctrl Pts',(3.26457513110646,2.08166817117217E-17,
23.3));
#6591=CARTESIAN_POINT('',(2.71715728752538,0.1,22.7171572875254));
#6592=CARTESIAN_POINT('Origin',(3.,0.1,23.));
#6593=CARTESIAN_POINT('Ctrl Pts',(2.6,-0.300000000000001,23.));
#6594=CARTESIAN_POINT('Ctrl Pts',(2.6,-0.300000000000001,22.9605580531743));
#6595=CARTESIAN_POINT('Ctrl Pts',(2.60628603952013,-0.291765800294272,22.9195707469402));
#6596=CARTESIAN_POINT('Ctrl Pts',(2.62882756515854,-0.260548600882862,22.8460176444472));
#6597=CARTESIAN_POINT('Ctrl Pts',(2.64492844776862,-0.237637949853888,22.813373881142));
#6598=CARTESIAN_POINT('Ctrl Pts',(2.67718134717306,-0.186078125959879,22.7618140572479));
#6599=CARTESIAN_POINT('Ctrl Pts',(2.69593643019745,-0.153499080170581,22.7392312552828));
#6600=CARTESIAN_POINT('Ctrl Pts',(2.71802972961529,-0.0989142979472494,
22.7160871167464));
#6601=CARTESIAN_POINT('Ctrl Pts',(2.7243365294397,-0.079743659916833,22.7100951351432));
#6602=CARTESIAN_POINT('Ctrl Pts',(2.73305334341681,-0.0403635841555955,
22.7020492278835));
#6603=CARTESIAN_POINT('Ctrl Pts',(2.73542486889354,-0.0201446772150696,
22.7));
#6604=CARTESIAN_POINT('Ctrl Pts',(2.73542486889354,0.,22.7));
#6605=CARTESIAN_POINT('Ctrl Pts',(2.73542486889354,0.0201446772150696,22.7));
#6606=CARTESIAN_POINT('Ctrl Pts',(2.73305334341681,0.0403635841555971,22.7020492278835));
#6607=CARTESIAN_POINT('Ctrl Pts',(2.72568156078613,0.0736671924755587,22.7088536267775));
#6608=CARTESIAN_POINT('Ctrl Pts',(2.72174110592258,0.0870350037104566,22.7125734691282));
#6609=CARTESIAN_POINT('Ctrl Pts',(2.71715728752538,0.0999999999999998,22.7171572875254));
#6610=CARTESIAN_POINT('Origin',(3.,0.1,23.));
#6611=CARTESIAN_POINT('',(-5.1,0.1,22.7171572875254));
#6612=CARTESIAN_POINT('Origin',(3.,-1.6,23.));
#6613=CARTESIAN_POINT('',(1.8,-1.5,23.));
#6614=CARTESIAN_POINT('Origin',(3.,-1.5,23.));
#6615=CARTESIAN_POINT('',(1.8,-1.,23.));
#6616=CARTESIAN_POINT('',(1.8,-1.6,23.));
#6617=CARTESIAN_POINT('Origin',(3.,-1.,23.));
#6618=CARTESIAN_POINT('Origin',(3.,-1.,23.));
#6619=CARTESIAN_POINT('Origin',(0.,0.1,23.));
#6620=CARTESIAN_POINT('',(0.282842712474617,0.1,23.2828427124746));
#6621=CARTESIAN_POINT('',(-0.282842712474617,0.1,23.2828427124746));
#6622=CARTESIAN_POINT('',(-5.1,0.1,23.2828427124746));
#6623=CARTESIAN_POINT('Origin',(0.,0.1,23.));
#6624=CARTESIAN_POINT('Origin',(0.,-2.1,23.));
#6625=CARTESIAN_POINT('',(-0.4,-1.,23.));
#6626=CARTESIAN_POINT('Origin',(0.,-1.,23.));
#6627=CARTESIAN_POINT('',(-0.4,-0.300000000000001,23.));
#6628=CARTESIAN_POINT('',(-0.4,-2.1,23.));
#6629=CARTESIAN_POINT('',(-0.264575131106458,-4.49191417939589E-18,23.3));
#6630=CARTESIAN_POINT('Ctrl Pts',(-0.264575131106458,1.04083408558608E-16,
23.3));
#6631=CARTESIAN_POINT('Ctrl Pts',(-0.264575131106458,-0.0201446772150695,
23.3));
#6632=CARTESIAN_POINT('Ctrl Pts',(-0.266946656583192,-0.0403635841555969,
23.2979507721165));
#6633=CARTESIAN_POINT('Ctrl Pts',(-0.275663470560296,-0.0797436599168343,
23.2899048648568));
#6634=CARTESIAN_POINT('Ctrl Pts',(-0.281970270384707,-0.0989142979472496,
23.2839128832536));
#6635=CARTESIAN_POINT('Ctrl Pts',(-0.30406356980255,-0.153499080170581,
23.2607687447172));
#6636=CARTESIAN_POINT('Ctrl Pts',(-0.322818652826944,-0.186078125959879,
23.2381859427521));
#6637=CARTESIAN_POINT('Ctrl Pts',(-0.35507155223138,-0.237637949853888,
23.186626118858));
#6638=CARTESIAN_POINT('Ctrl Pts',(-0.371172434841458,-0.260548600882862,
23.1539823555528));
#6639=CARTESIAN_POINT('Ctrl Pts',(-0.393713960479866,-0.291765800294272,
23.0804292530598));
#6640=CARTESIAN_POINT('Ctrl Pts',(-0.4,-0.300000000000001,23.0394419468257));
#6641=CARTESIAN_POINT('Ctrl Pts',(-0.4,-0.300000000000001,23.));
#6642=CARTESIAN_POINT('Ctrl Pts',(-0.282842712474619,0.099999999999999,
23.2828427124746));
#6643=CARTESIAN_POINT('Ctrl Pts',(-0.278258894172666,0.087035003979848,
23.2874265307766));
#6644=CARTESIAN_POINT('Ctrl Pts',(-0.274318439164031,0.0736671922504069,
23.2911463732685));
#6645=CARTESIAN_POINT('Ctrl Pts',(-0.266946656583192,0.0403635841555971,
23.2979507721165));
#6646=CARTESIAN_POINT('Ctrl Pts',(-0.264575131106458,0.0201446772150696,
23.3));
#6647=CARTESIAN_POINT('Ctrl Pts',(-0.264575131106458,-2.08166817117217E-17,
23.3));
#6648=CARTESIAN_POINT('',(0.264575131106458,1.11205971043954E-17,23.3));
#6649=CARTESIAN_POINT('Ctrl Pts',(0.264575131106458,-7.63278329429795E-17,
23.3));
#6650=CARTESIAN_POINT('Ctrl Pts',(0.264575131106458,0.0201446772150695,
23.3));
#6651=CARTESIAN_POINT('Ctrl Pts',(0.266946656583192,0.0403635841555971,
23.2979507721165));
#6652=CARTESIAN_POINT('Ctrl Pts',(0.274318439213869,0.0736671924755586,
23.2911463732225));
#6653=CARTESIAN_POINT('Ctrl Pts',(0.278258894077421,0.0870350037104561,
23.2874265308718));
#6654=CARTESIAN_POINT('Ctrl Pts',(0.282842712474618,0.0999999999999992,
23.2828427124746));
#6655=CARTESIAN_POINT('',(0.282842712474617,0.1,22.7171572875254));
#6656=CARTESIAN_POINT('Ctrl Pts',(0.282842712474619,0.1,22.7171572875254));
#6657=CARTESIAN_POINT('Ctrl Pts',(0.278258894172666,0.0870350039798482,
22.7125734692234));
#6658=CARTESIAN_POINT('Ctrl Pts',(0.274318439164031,0.0736671922504066,
22.7088536267315));
#6659=CARTESIAN_POINT('Ctrl Pts',(0.266946656583192,0.0403635841555971,
22.7020492278835));
#6660=CARTESIAN_POINT('Ctrl Pts',(0.264575131106458,0.0201446772150696,
22.7));
#6661=CARTESIAN_POINT('Ctrl Pts',(0.264575131106458,0.,22.7));
#6662=CARTESIAN_POINT('Ctrl Pts',(0.264575131106458,-0.0201446772150696,
22.7));
#6663=CARTESIAN_POINT('Ctrl Pts',(0.266946656583192,-0.0403635841555971,
22.7020492278835));
#6664=CARTESIAN_POINT('Ctrl Pts',(0.275663470560296,-0.0797436599168345,
22.7100951351432));
#6665=CARTESIAN_POINT('Ctrl Pts',(0.281970270384707,-0.0989142979472497,
22.7160871167464));
#6666=CARTESIAN_POINT('Ctrl Pts',(0.30406356980255,-0.153499080170581,22.7392312552828));
#6667=CARTESIAN_POINT('Ctrl Pts',(0.322818652826944,-0.186078125959879,
22.7618140572479));
#6668=CARTESIAN_POINT('Ctrl Pts',(0.35507155223138,-0.237637949853888,22.813373881142));
#6669=CARTESIAN_POINT('Ctrl Pts',(0.371172434841456,-0.260548600882859,
22.8460176444472));
#6670=CARTESIAN_POINT('Ctrl Pts',(0.393713960479865,-0.291765800294271,
22.9195707469402));
#6671=CARTESIAN_POINT('Ctrl Pts',(0.4,-0.300000000000001,22.9605580531743));
#6672=CARTESIAN_POINT('Ctrl Pts',(0.4,-0.300000000000001,23.0394419468257));
#6673=CARTESIAN_POINT('Ctrl Pts',(0.393713960479866,-0.291765800294272,
23.0804292530598));
#6674=CARTESIAN_POINT('Ctrl Pts',(0.371172434841458,-0.260548600882862,
23.1539823555528));
#6675=CARTESIAN_POINT('Ctrl Pts',(0.35507155223138,-0.237637949853888,23.186626118858));
#6676=CARTESIAN_POINT('Ctrl Pts',(0.322818652826944,-0.186078125959879,
23.2381859427521));
#6677=CARTESIAN_POINT('Ctrl Pts',(0.304063569802549,-0.153499080170581,
23.2607687447172));
#6678=CARTESIAN_POINT('Ctrl Pts',(0.281970270384707,-0.0989142979472497,
23.2839128832536));
#6679=CARTESIAN_POINT('Ctrl Pts',(0.275663470560296,-0.0797436599168345,
23.2899048648568));
#6680=CARTESIAN_POINT('Ctrl Pts',(0.266946656583192,-0.0403635841555971,
23.2979507721165));
#6681=CARTESIAN_POINT('Ctrl Pts',(0.264575131106458,-0.0201446772150695,
23.3));
#6682=CARTESIAN_POINT('Ctrl Pts',(0.264575131106458,8.67361737988404E-17,
23.3));
#6683=CARTESIAN_POINT('',(-0.282842712474617,0.1,22.7171572875254));
#6684=CARTESIAN_POINT('Origin',(0.,0.1,23.));
#6685=CARTESIAN_POINT('Ctrl Pts',(-0.4,-0.300000000000001,23.));
#6686=CARTESIAN_POINT('Ctrl Pts',(-0.4,-0.300000000000001,22.9605580531743));
#6687=CARTESIAN_POINT('Ctrl Pts',(-0.393713960479866,-0.291765800294272,
22.9195707469402));
#6688=CARTESIAN_POINT('Ctrl Pts',(-0.371172434841458,-0.260548600882862,
22.8460176444472));
#6689=CARTESIAN_POINT('Ctrl Pts',(-0.35507155223138,-0.237637949853888,
22.813373881142));
#6690=CARTESIAN_POINT('Ctrl Pts',(-0.322818652826944,-0.186078125959879,
22.7618140572479));
#6691=CARTESIAN_POINT('Ctrl Pts',(-0.30406356980255,-0.153499080170581,
22.7392312552828));
#6692=CARTESIAN_POINT('Ctrl Pts',(-0.281970270384707,-0.0989142979472497,
22.7160871167464));
#6693=CARTESIAN_POINT('Ctrl Pts',(-0.275663470560296,-0.0797436599168337,
22.7100951351432));
#6694=CARTESIAN_POINT('Ctrl Pts',(-0.266946656583192,-0.0403635841555955,
22.7020492278835));
#6695=CARTESIAN_POINT('Ctrl Pts',(-0.264575131106458,-0.0201446772150697,
22.7));
#6696=CARTESIAN_POINT('Ctrl Pts',(-0.264575131106458,0.,22.7));
#6697=CARTESIAN_POINT('Ctrl Pts',(-0.264575131106458,0.0201446772150696,
22.7));
#6698=CARTESIAN_POINT('Ctrl Pts',(-0.266946656583192,0.0403635841555971,
22.7020492278835));
#6699=CARTESIAN_POINT('Ctrl Pts',(-0.274318439213869,0.0736671924755591,
22.7088536267775));
#6700=CARTESIAN_POINT('Ctrl Pts',(-0.27825889407742,0.087035003710456,22.7125734691282));
#6701=CARTESIAN_POINT('Ctrl Pts',(-0.282842712474618,0.0999999999999995,
22.7171572875254));
#6702=CARTESIAN_POINT('Origin',(0.,0.1,23.));
#6703=CARTESIAN_POINT('',(-5.1,0.1,22.7171572875254));
#6704=CARTESIAN_POINT('Origin',(0.,-1.6,23.));
#6705=CARTESIAN_POINT('',(-1.2,-1.5,23.));
#6706=CARTESIAN_POINT('Origin',(0.,-1.5,23.));
#6707=CARTESIAN_POINT('',(-1.2,-1.,23.));
#6708=CARTESIAN_POINT('',(-1.2,-1.6,23.));
#6709=CARTESIAN_POINT('Origin',(0.,-1.,23.));
#6710=CARTESIAN_POINT('Origin',(0.,-1.,23.));
#6711=CARTESIAN_POINT('Origin',(-3.,0.1,23.));
#6712=CARTESIAN_POINT('',(-2.71715728752538,0.1,23.2828427124746));
#6713=CARTESIAN_POINT('',(-3.28284271247462,0.1,23.2828427124746));
#6714=CARTESIAN_POINT('',(-5.1,0.1,23.2828427124746));
#6715=CARTESIAN_POINT('Origin',(-3.,0.1,23.));
#6716=CARTESIAN_POINT('Origin',(-3.,-2.1,23.));
#6717=CARTESIAN_POINT('',(-3.4,-1.,23.));
#6718=CARTESIAN_POINT('Origin',(-3.,-1.,23.));
#6719=CARTESIAN_POINT('',(-3.4,-0.300000000000001,23.));
#6720=CARTESIAN_POINT('',(-3.4,-2.1,23.));
#6721=CARTESIAN_POINT('',(-3.26457513110646,-2.75719070341908E-18,23.3));
#6722=CARTESIAN_POINT('Ctrl Pts',(-3.26457513110646,1.14491749414469E-16,
23.3));
#6723=CARTESIAN_POINT('Ctrl Pts',(-3.26457513110646,-0.0201446772150695,
23.3));
#6724=CARTESIAN_POINT('Ctrl Pts',(-3.26694665658319,-0.0403635841555969,
23.2979507721165));
#6725=CARTESIAN_POINT('Ctrl Pts',(-3.27566347056029,-0.0797436599168342,
23.2899048648568));
#6726=CARTESIAN_POINT('Ctrl Pts',(-3.28197027038471,-0.0989142979472495,
23.2839128832536));
#6727=CARTESIAN_POINT('Ctrl Pts',(-3.30406356980255,-0.153499080170581,
23.2607687447172));
#6728=CARTESIAN_POINT('Ctrl Pts',(-3.32281865282694,-0.186078125959879,
23.2381859427521));
#6729=CARTESIAN_POINT('Ctrl Pts',(-3.35507155223138,-0.237637949853887,
23.186626118858));
#6730=CARTESIAN_POINT('Ctrl Pts',(-3.37117243484146,-0.260548600882861,
23.1539823555528));
#6731=CARTESIAN_POINT('Ctrl Pts',(-3.39371396047987,-0.291765800294272,
23.0804292530598));
#6732=CARTESIAN_POINT('Ctrl Pts',(-3.4,-0.300000000000001,23.0394419468257));
#6733=CARTESIAN_POINT('Ctrl Pts',(-3.4,-0.300000000000001,23.));
#6734=CARTESIAN_POINT('Ctrl Pts',(-3.28284271247462,0.0999999999999976,
23.2828427124746));
#6735=CARTESIAN_POINT('Ctrl Pts',(-3.27825889417267,0.0870350039798463,
23.2874265307766));
#6736=CARTESIAN_POINT('Ctrl Pts',(-3.27431843916403,0.0736671922504077,
23.2911463732685));
#6737=CARTESIAN_POINT('Ctrl Pts',(-3.26694665658319,0.0403635841555971,
23.2979507721165));
#6738=CARTESIAN_POINT('Ctrl Pts',(-3.26457513110646,0.0201446772150696,
23.3));
#6739=CARTESIAN_POINT('Ctrl Pts',(-3.26457513110646,-1.38777878078145E-17,
23.3));
#6740=CARTESIAN_POINT('',(-2.73542486889354,8.57137065713981E-17,23.3));
#6741=CARTESIAN_POINT('Ctrl Pts',(-2.73542486889354,9.36750677027476E-17,
23.3));
#6742=CARTESIAN_POINT('Ctrl Pts',(-2.73542486889354,0.0201446772150697,
23.3));
#6743=CARTESIAN_POINT('Ctrl Pts',(-2.73305334341681,0.0403635841555968,
23.2979507721165));
#6744=CARTESIAN_POINT('Ctrl Pts',(-2.72568156078613,0.0736671924755579,
23.2911463732225));
#6745=CARTESIAN_POINT('Ctrl Pts',(-2.72174110592258,0.0870350037104556,
23.2874265308718));
#6746=CARTESIAN_POINT('Ctrl Pts',(-2.71715728752538,0.0999999999999993,
23.2828427124746));
#6747=CARTESIAN_POINT('',(-2.71715728752538,0.1,22.7171572875254));
#6748=CARTESIAN_POINT('Ctrl Pts',(-2.71715728752538,0.0999999999999998,
22.7171572875254));
#6749=CARTESIAN_POINT('Ctrl Pts',(-2.72174110582733,0.0870350039798475,
22.7125734692234));
#6750=CARTESIAN_POINT('Ctrl Pts',(-2.72568156083597,0.0736671922504053,
22.7088536267315));
#6751=CARTESIAN_POINT('Ctrl Pts',(-2.73305334341681,0.0403635841555956,
22.7020492278835));
#6752=CARTESIAN_POINT('Ctrl Pts',(-2.73542486889354,0.0201446772150696,
22.7));
#6753=CARTESIAN_POINT('Ctrl Pts',(-2.73542486889354,0.,22.7));
#6754=CARTESIAN_POINT('Ctrl Pts',(-2.73542486889354,-0.0201446772150696,
22.7));
#6755=CARTESIAN_POINT('Ctrl Pts',(-2.73305334341681,-0.0403635841555972,
22.7020492278835));
#6756=CARTESIAN_POINT('Ctrl Pts',(-2.72433652943971,-0.0797436599168346,
22.7100951351432));
#6757=CARTESIAN_POINT('Ctrl Pts',(-2.71802972961529,-0.0989142979472495,
22.7160871167464));
#6758=CARTESIAN_POINT('Ctrl Pts',(-2.69593643019745,-0.153499080170581,
22.7392312552828));
#6759=CARTESIAN_POINT('Ctrl Pts',(-2.67718134717306,-0.186078125959879,
22.7618140572479));
#6760=CARTESIAN_POINT('Ctrl Pts',(-2.64492844776862,-0.237637949853888,
22.813373881142));
#6761=CARTESIAN_POINT('Ctrl Pts',(-2.62882756515854,-0.260548600882862,
22.8460176444472));
#6762=CARTESIAN_POINT('Ctrl Pts',(-2.60628603952013,-0.291765800294272,
22.9195707469402));
#6763=CARTESIAN_POINT('Ctrl Pts',(-2.6,-0.300000000000001,22.9605580531743));
#6764=CARTESIAN_POINT('Ctrl Pts',(-2.6,-0.300000000000001,23.0394419468257));
#6765=CARTESIAN_POINT('Ctrl Pts',(-2.60628603952013,-0.291765800294272,
23.0804292530598));
#6766=CARTESIAN_POINT('Ctrl Pts',(-2.62882756515854,-0.260548600882861,
23.1539823555528));
#6767=CARTESIAN_POINT('Ctrl Pts',(-2.64492844776862,-0.237637949853888,
23.186626118858));
#6768=CARTESIAN_POINT('Ctrl Pts',(-2.67718134717306,-0.186078125959879,
23.2381859427521));
#6769=CARTESIAN_POINT('Ctrl Pts',(-2.69593643019745,-0.153499080170581,
23.2607687447172));
#6770=CARTESIAN_POINT('Ctrl Pts',(-2.71802972961529,-0.0989142979472495,
23.2839128832536));
#6771=CARTESIAN_POINT('Ctrl Pts',(-2.72433652943971,-0.0797436599168343,
23.2899048648568));
#6772=CARTESIAN_POINT('Ctrl Pts',(-2.73305334341681,-0.0403635841555968,
23.2979507721165));
#6773=CARTESIAN_POINT('Ctrl Pts',(-2.73542486889354,-0.0201446772150696,
23.3));
#6774=CARTESIAN_POINT('Ctrl Pts',(-2.73542486889354,3.29597460435593E-17,
23.3));
#6775=CARTESIAN_POINT('',(-3.28284271247462,0.1,22.7171572875254));
#6776=CARTESIAN_POINT('Origin',(-3.,0.1,23.));
#6777=CARTESIAN_POINT('Ctrl Pts',(-3.4,-0.300000000000001,23.));
#6778=CARTESIAN_POINT('Ctrl Pts',(-3.4,-0.300000000000001,22.9605580531743));
#6779=CARTESIAN_POINT('Ctrl Pts',(-3.39371396047987,-0.291765800294272,
22.9195707469402));
#6780=CARTESIAN_POINT('Ctrl Pts',(-3.37117243484146,-0.260548600882862,
22.8460176444472));
#6781=CARTESIAN_POINT('Ctrl Pts',(-3.35507155223138,-0.237637949853888,
22.813373881142));
#6782=CARTESIAN_POINT('Ctrl Pts',(-3.32281865282694,-0.186078125959879,
22.7618140572479));
#6783=CARTESIAN_POINT('Ctrl Pts',(-3.30406356980255,-0.153499080170581,
22.7392312552828));
#6784=CARTESIAN_POINT('Ctrl Pts',(-3.28197027038471,-0.0989142979472495,
22.7160871167464));
#6785=CARTESIAN_POINT('Ctrl Pts',(-3.27566347056029,-0.0797436599168329,
22.7100951351432));
#6786=CARTESIAN_POINT('Ctrl Pts',(-3.26694665658319,-0.0403635841555953,
22.7020492278835));
#6787=CARTESIAN_POINT('Ctrl Pts',(-3.26457513110646,-0.0201446772150696,
22.7));
#6788=CARTESIAN_POINT('Ctrl Pts',(-3.26457513110646,0.,22.7));
#6789=CARTESIAN_POINT('Ctrl Pts',(-3.26457513110646,0.0201446772150696,
22.7));
#6790=CARTESIAN_POINT('Ctrl Pts',(-3.26694665658319,0.0403635841555971,
22.7020492278835));
#6791=CARTESIAN_POINT('Ctrl Pts',(-3.27431843921387,0.0736671924755593,
22.7088536267775));
#6792=CARTESIAN_POINT('Ctrl Pts',(-3.27825889407742,0.0870350037104561,
22.7125734691282));
#6793=CARTESIAN_POINT('Ctrl Pts',(-3.28284271247462,0.0999999999999997,
22.7171572875254));
#6794=CARTESIAN_POINT('Origin',(-3.,0.1,23.));
#6795=CARTESIAN_POINT('',(-5.1,0.1,22.7171572875254));
#6796=CARTESIAN_POINT('Origin',(-3.,-1.6,23.));
#6797=CARTESIAN_POINT('',(-4.2,-1.5,23.));
#6798=CARTESIAN_POINT('Origin',(-3.,-1.5,23.));
#6799=CARTESIAN_POINT('',(-4.2,-1.,23.));
#6800=CARTESIAN_POINT('',(-4.2,-1.6,23.));
#6801=CARTESIAN_POINT('Origin',(-3.,-1.,23.));
#6802=CARTESIAN_POINT('Origin',(-3.,-1.,23.));
#6803=CARTESIAN_POINT('Origin',(3.6,0.,23.));
#6804=CARTESIAN_POINT('',(3.6,-8.38883057415935E-17,23.685));
#6805=CARTESIAN_POINT('Origin',(3.6,0.,23.));
#6806=CARTESIAN_POINT('',(5.,8.38883057415935E-17,23.685));
#6807=CARTESIAN_POINT('',(3.6,-8.38883057415935E-17,23.685));
#6808=CARTESIAN_POINT('Origin',(5.,0.,23.));
#6809=CARTESIAN_POINT('',(4.3,0.6,23.3304920573932));
#6810=CARTESIAN_POINT('Ctrl Pts',(4.3,0.6,23.3304920573932));
#6811=CARTESIAN_POINT('Ctrl Pts',(4.27077753133383,0.6,23.3304920573932));
#6812=CARTESIAN_POINT('Ctrl Pts',(4.24011034888269,0.603494484869573,23.3243525399112));
#6813=CARTESIAN_POINT('Ctrl Pts',(4.18479795469579,0.615901327435478,23.3001263251791));
#6814=CARTESIAN_POINT('Ctrl Pts',(4.16014428890256,0.624655274357919,23.2819781026066));
#6815=CARTESIAN_POINT('Ctrl Pts',(4.12028928729214,0.641942325510241,23.2401640721199));
#6816=CARTESIAN_POINT('Ctrl Pts',(4.10113513579261,0.652637676126791,23.2100112664292));
#6817=CARTESIAN_POINT('Ctrl Pts',(4.07712932095812,0.667553927651758,23.1560425561636));
#6818=CARTESIAN_POINT('Ctrl Pts',(4.06787168700093,0.674162120990136,23.1254789195617));
#6819=CARTESIAN_POINT('Ctrl Pts',(4.05607440793796,0.682897228967308,23.0623771974352));
#6820=CARTESIAN_POINT('Ctrl Pts',(4.05347413928758,0.684999999999999,23.0298471208273));
#6821=CARTESIAN_POINT('Ctrl Pts',(4.05347413928758,0.684999999999999,22.9701528791727));
#6822=CARTESIAN_POINT('Ctrl Pts',(4.05607440793796,0.682897228967308,22.9376228025648));
#6823=CARTESIAN_POINT('Ctrl Pts',(4.06787168700092,0.674162120990137,22.8745210804384));
#6824=CARTESIAN_POINT('Ctrl Pts',(4.07712932095812,0.667553927651758,22.8439574438364));
#6825=CARTESIAN_POINT('Ctrl Pts',(4.10113513579261,0.652637676126791,22.7899887335708));
#6826=CARTESIAN_POINT('Ctrl Pts',(4.12028928729214,0.641942325510241,22.7598359278801));
#6827=CARTESIAN_POINT('Ctrl Pts',(4.16014428890256,0.624655274357919,22.7180218973934));
#6828=CARTESIAN_POINT('Ctrl Pts',(4.18479795469579,0.615901327435478,22.6998736748209));
#6829=CARTESIAN_POINT('Ctrl Pts',(4.24011034888269,0.603494484869573,22.6756474600888));
#6830=CARTESIAN_POINT('Ctrl Pts',(4.27077753133383,0.6,22.6695079426068));
#6831=CARTESIAN_POINT('Ctrl Pts',(4.32922246866617,0.6,22.6695079426068));
#6832=CARTESIAN_POINT('Ctrl Pts',(4.3598896511173,0.603494484869573,22.6756474600888));
#6833=CARTESIAN_POINT('Ctrl Pts',(4.41520204530421,0.615901327435478,22.6998736748209));
#6834=CARTESIAN_POINT('Ctrl Pts',(4.43985571109744,0.624655274357919,22.7180218973934));
#6835=CARTESIAN_POINT('Ctrl Pts',(4.47971071270786,0.641942325510241,22.7598359278801));
#6836=CARTESIAN_POINT('Ctrl Pts',(4.49886486420739,0.652637676126791,22.7899887335708));
#6837=CARTESIAN_POINT('Ctrl Pts',(4.52287067904188,0.667553927651758,22.8439574438364));
#6838=CARTESIAN_POINT('Ctrl Pts',(4.53212831299907,0.674162120990137,22.8745210804384));
#6839=CARTESIAN_POINT('Ctrl Pts',(4.54392559206204,0.682897228967308,22.9376228025648));
#6840=CARTESIAN_POINT('Ctrl Pts',(4.54652586071242,0.684999999999999,22.9701528791727));
#6841=CARTESIAN_POINT('Ctrl Pts',(4.54652586071242,0.684999999999999,23.0298471208273));
#6842=CARTESIAN_POINT('Ctrl Pts',(4.54392559206204,0.682897228967308,23.0623771974352));
#6843=CARTESIAN_POINT('Ctrl Pts',(4.53212831299907,0.674162120990136,23.1254789195617));
#6844=CARTESIAN_POINT('Ctrl Pts',(4.52287067904188,0.667553927651758,23.1560425561636));
#6845=CARTESIAN_POINT('Ctrl Pts',(4.49886486420739,0.652637676126791,23.2100112664292));
#6846=CARTESIAN_POINT('Ctrl Pts',(4.47971071270786,0.641942325510241,23.2401640721199));
#6847=CARTESIAN_POINT('Ctrl Pts',(4.43985571109744,0.624655274357919,23.2819781026066));
#6848=CARTESIAN_POINT('Ctrl Pts',(4.41520204530421,0.615901327435478,23.3001263251791));
#6849=CARTESIAN_POINT('Ctrl Pts',(4.3598896511173,0.603494484869573,23.3243525399112));
#6850=CARTESIAN_POINT('Ctrl Pts',(4.32922246866617,0.6,23.3304920573932));
#6851=CARTESIAN_POINT('Ctrl Pts',(4.3,0.6,23.3304920573932));
#6852=CARTESIAN_POINT('Origin',(3.6,0.,23.));
#6853=CARTESIAN_POINT('',(3.6,-3.67394039744207E-17,23.3));
#6854=CARTESIAN_POINT('Origin',(3.6,0.,23.));
#6855=CARTESIAN_POINT('Origin',(-5.1,0.,23.));
#6856=CARTESIAN_POINT('',(-5.,-3.67394039744207E-17,23.3));
#6857=CARTESIAN_POINT('Origin',(-5.,0.,23.));
#6858=CARTESIAN_POINT('',(-5.1,-3.67394039744207E-17,23.3));
#6859=CARTESIAN_POINT('',(-5.1,-3.67394039744207E-17,23.3));
#6860=CARTESIAN_POINT('',(-5.1,-3.67394039744207E-17,23.3));
#6861=CARTESIAN_POINT('',(-5.1,-3.67394039744207E-17,23.3));
#6862=CARTESIAN_POINT('Origin',(-4.3,1.,22.3));
#6863=CARTESIAN_POINT('',(-4.7,1.,22.3));
#6864=CARTESIAN_POINT('Origin',(-4.3,1.,22.3));
#6865=CARTESIAN_POINT('',(-4.7,1.,24.5));
#6866=CARTESIAN_POINT('',(-4.7,1.,22.3));
#6867=CARTESIAN_POINT('Origin',(-4.3,1.,24.5));
#6868=CARTESIAN_POINT('Origin',(-4.3,1.,22.3));
#6869=CARTESIAN_POINT('',(-4.525,1.,22.3));
#6870=CARTESIAN_POINT('Origin',(-4.3,1.,22.3));
#6871=CARTESIAN_POINT('Origin',(4.3,1.,22.3));
#6872=CARTESIAN_POINT('',(3.9,1.,22.3));
#6873=CARTESIAN_POINT('Origin',(4.3,1.,22.3));
#6874=CARTESIAN_POINT('',(3.9,1.,24.5));
#6875=CARTESIAN_POINT('',(3.9,1.,22.3));
#6876=CARTESIAN_POINT('Origin',(4.3,1.,24.5));
#6877=CARTESIAN_POINT('Origin',(4.3,1.,22.3));
#6878=CARTESIAN_POINT('',(4.075,1.,22.3));
#6879=CARTESIAN_POINT('Origin',(4.3,1.,22.3));
#6880=CARTESIAN_POINT('Origin',(-4.3,1.,21.4));
#6881=CARTESIAN_POINT('',(-4.525,1.,21.5));
#6882=CARTESIAN_POINT('Origin',(-4.3,1.,21.5));
#6883=CARTESIAN_POINT('',(-4.525,1.,21.4));
#6884=CARTESIAN_POINT('Origin',(4.3,1.,21.4));
#6885=CARTESIAN_POINT('',(4.075,1.,21.5));
#6886=CARTESIAN_POINT('Origin',(4.3,1.,21.5));
#6887=CARTESIAN_POINT('',(4.075,1.,21.4));
#6888=CARTESIAN_POINT('Origin',(5.,1.5,21.5));
#6889=CARTESIAN_POINT('',(5.,1.5,21.5));
#6890=CARTESIAN_POINT('',(-5.,1.5,21.5));
#6891=CARTESIAN_POINT('',(5.,1.5,21.5));
#6892=CARTESIAN_POINT('',(-5.,1.5,24.5));
#6893=CARTESIAN_POINT('',(-5.,1.5,21.5));
#6894=CARTESIAN_POINT('',(5.,1.5,24.5));
#6895=CARTESIAN_POINT('',(5.,1.5,24.5));
#6896=CARTESIAN_POINT('',(5.,1.5,21.5));
#6897=CARTESIAN_POINT('Origin',(5.,-1.5,21.5));
#6898=CARTESIAN_POINT('',(5.,-1.5,21.5));
#6899=CARTESIAN_POINT('',(5.,-1.5,21.5));
#6900=CARTESIAN_POINT('',(5.,-1.5,24.5));
#6901=CARTESIAN_POINT('',(5.,-1.5,24.5));
#6902=CARTESIAN_POINT('',(5.,-1.5,21.5));
#6903=CARTESIAN_POINT('Origin',(-5.,-1.5,21.5));
#6904=CARTESIAN_POINT('',(-5.,-1.5,21.5));
#6905=CARTESIAN_POINT('',(-5.,-1.5,21.5));
#6906=CARTESIAN_POINT('',(-5.,-1.5,24.5));
#6907=CARTESIAN_POINT('',(-5.,-1.5,24.5));
#6908=CARTESIAN_POINT('',(-5.,-1.5,21.5));
#6909=CARTESIAN_POINT('Origin',(-5.,1.5,21.5));
#6910=CARTESIAN_POINT('',(-5.,1.5,21.5));
#6911=CARTESIAN_POINT('',(-5.,1.5,24.5));
#6912=CARTESIAN_POINT('Origin',(0.,0.,24.5));
#6913=CARTESIAN_POINT('Origin',(0.,0.,21.5));
#6914=CARTESIAN_POINT('',(0.,0.,0.));
#6915=CARTESIAN_POINT('Origin',(-5.,0.,23.));
#6916=CARTESIAN_POINT('',(-4.6,-3.67394039744207E-17,23.3));
#6917=CARTESIAN_POINT('Origin',(-4.6,0.,23.));
#6918=CARTESIAN_POINT('',(-5.,-3.67394039744207E-17,23.3));
#6919=CARTESIAN_POINT('',(-5.,-3.67394039744207E-17,23.3));
#6920=CARTESIAN_POINT('Origin',(-5.,0.,23.));
#6921=CARTESIAN_POINT('Origin',(-4.6,0.,23.));
#6922=CARTESIAN_POINT('Origin',(-5.,0.,23.));
#6923=CARTESIAN_POINT('',(0.,0.,0.));
#6924=CARTESIAN_POINT('Origin',(-3.,-2.1,23.));
#6925=CARTESIAN_POINT('',(-3.4,-1.08348486100883,23.));
#6926=CARTESIAN_POINT('Origin',(-3.,-1.08348486100883,23.));
#6927=CARTESIAN_POINT('',(-3.4,-1.,23.));
#6928=CARTESIAN_POINT('',(-3.4,-2.1,23.));
#6929=CARTESIAN_POINT('Origin',(-3.,-1.,23.));
#6930=CARTESIAN_POINT('Origin',(-3.,-3.3,23.));
#6931=CARTESIAN_POINT('',(-3.85,-3.2,23.));
#6932=CARTESIAN_POINT('Origin',(-3.,-3.2,23.));
#6933=CARTESIAN_POINT('',(-3.85,-2.52678268764264,23.));
#6934=CARTESIAN_POINT('',(-3.85,-3.3,23.));
#6935=CARTESIAN_POINT('Origin',(-3.,-2.52678268764264,23.));
#6936=CARTESIAN_POINT('Origin',(-3.,-2.,23.));
#6937=CARTESIAN_POINT('',(-3.,-2.,22.));
#6938=CARTESIAN_POINT('',(-3.,-2.,24.));
#6939=CARTESIAN_POINT('Origin',(-3.,-2.,23.));
#6940=CARTESIAN_POINT('Origin',(-3.,-1.5,23.));
#6941=CARTESIAN_POINT('',(-4.2,-1.,23.));
#6942=CARTESIAN_POINT('Origin',(-3.,-1.,23.));
#6943=CARTESIAN_POINT('',(-4.2,-1.5,23.));
#6944=CARTESIAN_POINT('',(-4.2,-1.5,23.));
#6945=CARTESIAN_POINT('Origin',(-3.,-1.5,23.));
#6946=CARTESIAN_POINT('Origin',(-3.,-1.,23.));
#6947=CARTESIAN_POINT('Origin',(-3.,-3.2,23.));
#6948=CARTESIAN_POINT('',(-4.4,-1.5,23.));
#6949=CARTESIAN_POINT('Origin',(-3.,-1.5,23.));
#6950=CARTESIAN_POINT('',(-4.4,-3.2,23.));
#6951=CARTESIAN_POINT('',(-4.4,-3.2,23.));
#6952=CARTESIAN_POINT('Origin',(-3.,-3.2,23.));
#6953=CARTESIAN_POINT('Origin',(-3.,-1.5,23.));
#6954=CARTESIAN_POINT('Origin',(-3.,-3.2,23.));
#6955=CARTESIAN_POINT('',(0.,0.,0.));
#6956=CARTESIAN_POINT('Origin',(0.,-2.1,23.));
#6957=CARTESIAN_POINT('',(-0.4,-1.08348486100883,23.));
#6958=CARTESIAN_POINT('Origin',(0.,-1.08348486100883,23.));
#6959=CARTESIAN_POINT('',(-0.4,-1.,23.));
#6960=CARTESIAN_POINT('',(-0.4,-2.1,23.));
#6961=CARTESIAN_POINT('Origin',(0.,-1.,23.));
#6962=CARTESIAN_POINT('Origin',(0.,-3.3,23.));
#6963=CARTESIAN_POINT('',(-0.85,-3.2,23.));
#6964=CARTESIAN_POINT('Origin',(0.,-3.2,23.));
#6965=CARTESIAN_POINT('',(-0.85,-2.52678268764264,23.));
#6966=CARTESIAN_POINT('',(-0.85,-3.3,23.));
#6967=CARTESIAN_POINT('Origin',(0.,-2.52678268764264,23.));
#6968=CARTESIAN_POINT('Origin',(0.,-2.,23.));
#6969=CARTESIAN_POINT('',(-6.12323399573677E-17,-2.,22.));
#6970=CARTESIAN_POINT('',(-6.12323399573677E-17,-2.,24.));
#6971=CARTESIAN_POINT('Origin',(0.,-2.,23.));
#6972=CARTESIAN_POINT('Origin',(0.,-1.5,23.));
#6973=CARTESIAN_POINT('',(-1.2,-1.,23.));
#6974=CARTESIAN_POINT('Origin',(0.,-1.,23.));
#6975=CARTESIAN_POINT('',(-1.2,-1.5,23.));
#6976=CARTESIAN_POINT('',(-1.2,-1.5,23.));
#6977=CARTESIAN_POINT('Origin',(0.,-1.5,23.));
#6978=CARTESIAN_POINT('Origin',(0.,-1.,23.));
#6979=CARTESIAN_POINT('Origin',(0.,-3.2,23.));
#6980=CARTESIAN_POINT('',(-1.4,-1.5,23.));
#6981=CARTESIAN_POINT('Origin',(0.,-1.5,23.));
#6982=CARTESIAN_POINT('',(-1.4,-3.2,23.));
#6983=CARTESIAN_POINT('',(-1.4,-3.2,23.));
#6984=CARTESIAN_POINT('Origin',(0.,-3.2,23.));
#6985=CARTESIAN_POINT('Origin',(0.,-1.5,23.));
#6986=CARTESIAN_POINT('Origin',(0.,-3.2,23.));
#6987=CARTESIAN_POINT('',(0.,0.,0.));
#6988=CARTESIAN_POINT('Origin',(3.,-2.1,23.));
#6989=CARTESIAN_POINT('',(2.6,-1.08348486100883,23.));
#6990=CARTESIAN_POINT('Origin',(3.,-1.08348486100883,23.));
#6991=CARTESIAN_POINT('',(2.6,-1.,23.));
#6992=CARTESIAN_POINT('',(2.6,-2.1,23.));
#6993=CARTESIAN_POINT('Origin',(3.,-1.,23.));
#6994=CARTESIAN_POINT('Origin',(3.,-3.3,23.));
#6995=CARTESIAN_POINT('',(2.15,-3.2,23.));
#6996=CARTESIAN_POINT('Origin',(3.,-3.2,23.));
#6997=CARTESIAN_POINT('',(2.15,-2.52678268764264,23.));
#6998=CARTESIAN_POINT('',(2.15,-3.3,23.));
#6999=CARTESIAN_POINT('Origin',(3.,-2.52678268764264,23.));
#7000=CARTESIAN_POINT('Origin',(3.,-2.,23.));
#7001=CARTESIAN_POINT('',(3.,-2.,22.));
#7002=CARTESIAN_POINT('',(3.,-2.,24.));
#7003=CARTESIAN_POINT('Origin',(3.,-2.,23.));
#7004=CARTESIAN_POINT('Origin',(3.,-1.5,23.));
#7005=CARTESIAN_POINT('',(1.8,-1.,23.));
#7006=CARTESIAN_POINT('Origin',(3.,-1.,23.));
#7007=CARTESIAN_POINT('',(1.8,-1.5,23.));
#7008=CARTESIAN_POINT('',(1.8,-1.5,23.));
#7009=CARTESIAN_POINT('Origin',(3.,-1.5,23.));
#7010=CARTESIAN_POINT('Origin',(3.,-1.,23.));
#7011=CARTESIAN_POINT('Origin',(3.,-3.2,23.));
#7012=CARTESIAN_POINT('',(1.6,-1.5,23.));
#7013=CARTESIAN_POINT('Origin',(3.,-1.5,23.));
#7014=CARTESIAN_POINT('',(1.6,-3.2,23.));
#7015=CARTESIAN_POINT('',(1.6,-3.2,23.));
#7016=CARTESIAN_POINT('Origin',(3.,-3.2,23.));
#7017=CARTESIAN_POINT('Origin',(3.,-1.5,23.));
#7018=CARTESIAN_POINT('Origin',(3.,-3.2,23.));
#7019=CARTESIAN_POINT('',(0.,0.,0.));
#7020=CARTESIAN_POINT('Origin',(-0.1,0.82,-0.3));
#7021=CARTESIAN_POINT('',(0.,0.82,-0.3));
#7022=CARTESIAN_POINT('',(0.,1.,-0.3));
#7023=CARTESIAN_POINT('',(0.,0.41,-0.3));
#7024=CARTESIAN_POINT('',(20.,0.82,-0.3));
#7025=CARTESIAN_POINT('',(-0.1,0.82,-0.3));
#7026=CARTESIAN_POINT('',(20.,1.,-0.3));
#7027=CARTESIAN_POINT('',(20.,0.41,-0.3));
#7028=CARTESIAN_POINT('',(-0.05,1.,-0.3));
#7029=CARTESIAN_POINT('Origin',(-0.1,0.82,-0.55));
#7030=CARTESIAN_POINT('',(0.,0.82,-0.55));
#7031=CARTESIAN_POINT('',(0.,0.82,-0.275));
#7032=CARTESIAN_POINT('',(20.,0.82,-0.55));
#7033=CARTESIAN_POINT('',(-0.1,0.82,-0.55));
#7034=CARTESIAN_POINT('',(20.,0.82,-0.275));
#7035=CARTESIAN_POINT('Origin',(-0.1,0.67,-0.55));
#7036=CARTESIAN_POINT('',(0.,0.67,-0.55));
#7037=CARTESIAN_POINT('',(0.,0.335,-0.55));
#7038=CARTESIAN_POINT('',(20.,0.67,-0.55));
#7039=CARTESIAN_POINT('',(-0.1,0.67,-0.55));
#7040=CARTESIAN_POINT('',(20.,0.335,-0.55));
#7041=CARTESIAN_POINT('Origin',(-0.1,0.42,-0.3));
#7042=CARTESIAN_POINT('',(0.,0.42,-0.3));
#7043=CARTESIAN_POINT('',(0.,0.24,-0.12));
#7044=CARTESIAN_POINT('',(20.,0.42,-0.3));
#7045=CARTESIAN_POINT('',(-0.1,0.42,-0.3));
#7046=CARTESIAN_POINT('',(20.,0.24,-0.12));
#7047=CARTESIAN_POINT('Origin',(-0.1,0.42,0.3));
#7048=CARTESIAN_POINT('',(0.,0.42,0.3));
#7049=CARTESIAN_POINT('',(0.,0.42,0.15));
#7050=CARTESIAN_POINT('',(20.,0.42,0.3));
#7051=CARTESIAN_POINT('',(-0.1,0.42,0.3));
#7052=CARTESIAN_POINT('',(20.,0.42,0.15));
#7053=CARTESIAN_POINT('Origin',(-0.1,0.67,0.55));
#7054=CARTESIAN_POINT('',(0.,0.67,0.55));
#7055=CARTESIAN_POINT('',(6.93889390390723E-18,0.365,0.245));
#7056=CARTESIAN_POINT('',(20.,0.67,0.55));
#7057=CARTESIAN_POINT('',(-0.1,0.67,0.55));
#7058=CARTESIAN_POINT('',(20.,0.365,0.245));
#7059=CARTESIAN_POINT('Origin',(-0.1,0.82,0.55));
#7060=CARTESIAN_POINT('',(0.,0.82,0.55));
#7061=CARTESIAN_POINT('',(0.,0.41,0.55));
#7062=CARTESIAN_POINT('',(20.,0.82,0.55));
#7063=CARTESIAN_POINT('',(-0.1,0.82,0.55));
#7064=CARTESIAN_POINT('',(20.,0.41,0.55));
#7065=CARTESIAN_POINT('Origin',(-0.1,0.82,0.3));
#7066=CARTESIAN_POINT('',(0.,0.82,0.3));
#7067=CARTESIAN_POINT('',(0.,0.82,0.15));
#7068=CARTESIAN_POINT('',(20.,0.82,0.3));
#7069=CARTESIAN_POINT('',(-0.1,0.82,0.3));
#7070=CARTESIAN_POINT('',(20.,0.82,0.15));
#7071=CARTESIAN_POINT('Origin',(-0.1,1.05,0.3));
#7072=CARTESIAN_POINT('',(0.,1.,0.3));
#7073=CARTESIAN_POINT('',(0.,0.525,0.3));
#7074=CARTESIAN_POINT('',(20.,1.,0.3));
#7075=CARTESIAN_POINT('',(-0.05,1.,0.3));
#7076=CARTESIAN_POINT('',(20.,0.525,0.3));
#7077=CARTESIAN_POINT('Origin',(-0.1,-0.3,-0.82));
#7078=CARTESIAN_POINT('',(0.,-0.3,-0.82));
#7079=CARTESIAN_POINT('',(0.,-0.3,-1.));
#7080=CARTESIAN_POINT('',(0.,-0.3,-0.41));
#7081=CARTESIAN_POINT('',(20.,-0.3,-0.82));
#7082=CARTESIAN_POINT('',(-0.1,-0.3,-0.82));
#7083=CARTESIAN_POINT('',(20.,-0.3,-1.));
#7084=CARTESIAN_POINT('',(20.,-0.3,-0.41));
#7085=CARTESIAN_POINT('',(-0.05,-0.3,-1.));
#7086=CARTESIAN_POINT('Origin',(-0.1,-0.55,-0.82));
#7087=CARTESIAN_POINT('',(0.,-0.55,-0.82));
#7088=CARTESIAN_POINT('',(0.,-0.275,-0.82));
#7089=CARTESIAN_POINT('',(20.,-0.55,-0.82));
#7090=CARTESIAN_POINT('',(-0.1,-0.55,-0.82));
#7091=CARTESIAN_POINT('',(20.,-0.275,-0.82));
#7092=CARTESIAN_POINT('Origin',(-0.1,-0.55,-0.67));
#7093=CARTESIAN_POINT('',(0.,-0.55,-0.67));
#7094=CARTESIAN_POINT('',(0.,-0.55,-0.335));
#7095=CARTESIAN_POINT('',(20.,-0.55,-0.67));
#7096=CARTESIAN_POINT('',(-0.1,-0.55,-0.67));
#7097=CARTESIAN_POINT('',(20.,-0.55,-0.335));
#7098=CARTESIAN_POINT('Origin',(-0.1,-0.3,-0.42));
#7099=CARTESIAN_POINT('',(0.,-0.3,-0.42));
#7100=CARTESIAN_POINT('',(0.,-0.12,-0.24));
#7101=CARTESIAN_POINT('',(20.,-0.3,-0.42));
#7102=CARTESIAN_POINT('',(-0.1,-0.3,-0.42));
#7103=CARTESIAN_POINT('',(20.,-0.12,-0.24));
#7104=CARTESIAN_POINT('Origin',(-0.1,0.3,-0.42));
#7105=CARTESIAN_POINT('',(0.,0.3,-0.42));
#7106=CARTESIAN_POINT('',(0.,0.15,-0.42));
#7107=CARTESIAN_POINT('',(20.,0.3,-0.42));
#7108=CARTESIAN_POINT('',(-0.1,0.3,-0.42));
#7109=CARTESIAN_POINT('',(20.,0.15,-0.42));
#7110=CARTESIAN_POINT('Origin',(-0.1,0.55,-0.67));
#7111=CARTESIAN_POINT('',(0.,0.55,-0.67));
#7112=CARTESIAN_POINT('',(0.,0.245,-0.365));
#7113=CARTESIAN_POINT('',(20.,0.55,-0.67));
#7114=CARTESIAN_POINT('',(-0.1,0.55,-0.67));
#7115=CARTESIAN_POINT('',(20.,0.245,-0.365));
#7116=CARTESIAN_POINT('Origin',(-0.1,0.55,-0.82));
#7117=CARTESIAN_POINT('',(0.,0.55,-0.82));
#7118=CARTESIAN_POINT('',(0.,0.55,-0.41));
#7119=CARTESIAN_POINT('',(20.,0.55,-0.82));
#7120=CARTESIAN_POINT('',(-0.1,0.55,-0.82));
#7121=CARTESIAN_POINT('',(20.,0.55,-0.41));
#7122=CARTESIAN_POINT('Origin',(-0.1,0.3,-0.82));
#7123=CARTESIAN_POINT('',(0.,0.3,-0.82));
#7124=CARTESIAN_POINT('',(0.,0.15,-0.82));
#7125=CARTESIAN_POINT('',(20.,0.3,-0.82));
#7126=CARTESIAN_POINT('',(-0.1,0.3,-0.82));
#7127=CARTESIAN_POINT('',(20.,0.15,-0.82));
#7128=CARTESIAN_POINT('Origin',(-0.1,0.3,-1.05));
#7129=CARTESIAN_POINT('',(0.,0.3,-1.));
#7130=CARTESIAN_POINT('',(0.,0.3,-0.525));
#7131=CARTESIAN_POINT('',(20.,0.3,-1.));
#7132=CARTESIAN_POINT('',(-0.05,0.3,-1.));
#7133=CARTESIAN_POINT('',(20.,0.3,-0.525));
#7134=CARTESIAN_POINT('Origin',(-0.1,-0.82,0.3));
#7135=CARTESIAN_POINT('',(0.,-0.82,0.3));
#7136=CARTESIAN_POINT('',(0.,-1.,0.3));
#7137=CARTESIAN_POINT('',(0.,-0.41,0.3));
#7138=CARTESIAN_POINT('',(20.,-0.82,0.3));
#7139=CARTESIAN_POINT('',(-0.1,-0.82,0.3));
#7140=CARTESIAN_POINT('',(20.,-1.,0.3));
#7141=CARTESIAN_POINT('',(20.,-0.41,0.3));
#7142=CARTESIAN_POINT('',(-0.05,-1.,0.3));
#7143=CARTESIAN_POINT('Origin',(-0.1,-0.82,0.55));
#7144=CARTESIAN_POINT('',(0.,-0.82,0.55));
#7145=CARTESIAN_POINT('',(0.,-0.82,0.275));
#7146=CARTESIAN_POINT('',(20.,-0.82,0.55));
#7147=CARTESIAN_POINT('',(-0.1,-0.82,0.55));
#7148=CARTESIAN_POINT('',(20.,-0.82,0.275));
#7149=CARTESIAN_POINT('Origin',(-0.1,-0.67,0.55));
#7150=CARTESIAN_POINT('',(0.,-0.67,0.55));
#7151=CARTESIAN_POINT('',(0.,-0.335,0.55));
#7152=CARTESIAN_POINT('',(20.,-0.67,0.55));
#7153=CARTESIAN_POINT('',(-0.1,-0.67,0.55));
#7154=CARTESIAN_POINT('',(20.,-0.335,0.55));
#7155=CARTESIAN_POINT('Origin',(-0.1,-0.42,0.3));
#7156=CARTESIAN_POINT('',(0.,-0.42,0.3));
#7157=CARTESIAN_POINT('',(-6.93889390390723E-18,-0.24,0.12));
#7158=CARTESIAN_POINT('',(20.,-0.42,0.3));
#7159=CARTESIAN_POINT('',(-0.1,-0.42,0.3));
#7160=CARTESIAN_POINT('',(20.,-0.24,0.12));
#7161=CARTESIAN_POINT('Origin',(-0.1,-0.42,-0.3));
#7162=CARTESIAN_POINT('',(0.,-0.42,-0.3));
#7163=CARTESIAN_POINT('',(0.,-0.42,-0.15));
#7164=CARTESIAN_POINT('',(20.,-0.42,-0.3));
#7165=CARTESIAN_POINT('',(-0.1,-0.42,-0.3));
#7166=CARTESIAN_POINT('',(20.,-0.42,-0.15));
#7167=CARTESIAN_POINT('Origin',(-0.1,-0.67,-0.55));
#7168=CARTESIAN_POINT('',(0.,-0.67,-0.55));
#7169=CARTESIAN_POINT('',(0.,-0.365,-0.245));
#7170=CARTESIAN_POINT('',(20.,-0.67,-0.55));
#7171=CARTESIAN_POINT('',(-0.1,-0.67,-0.55));
#7172=CARTESIAN_POINT('',(20.,-0.365,-0.245));
#7173=CARTESIAN_POINT('Origin',(-0.1,-0.82,-0.55));
#7174=CARTESIAN_POINT('',(0.,-0.82,-0.55));
#7175=CARTESIAN_POINT('',(0.,-0.41,-0.55));
#7176=CARTESIAN_POINT('',(20.,-0.82,-0.55));
#7177=CARTESIAN_POINT('',(-0.1,-0.82,-0.55));
#7178=CARTESIAN_POINT('',(20.,-0.41,-0.55));
#7179=CARTESIAN_POINT('Origin',(-0.1,-0.82,-0.3));
#7180=CARTESIAN_POINT('',(0.,-0.82,-0.3));
#7181=CARTESIAN_POINT('',(0.,-0.82,-0.15));
#7182=CARTESIAN_POINT('',(20.,-0.82,-0.3));
#7183=CARTESIAN_POINT('',(-0.1,-0.82,-0.3));
#7184=CARTESIAN_POINT('',(20.,-0.82,-0.15));
#7185=CARTESIAN_POINT('Origin',(-0.1,-1.05,-0.3));
#7186=CARTESIAN_POINT('',(0.,-1.,-0.3));
#7187=CARTESIAN_POINT('',(0.,-0.525,-0.3));
#7188=CARTESIAN_POINT('',(20.,-1.,-0.3));
#7189=CARTESIAN_POINT('',(-0.05,-1.,-0.3));
#7190=CARTESIAN_POINT('',(20.,-0.525,-0.3));
#7191=CARTESIAN_POINT('Origin',(-0.1,0.3,0.82));
#7192=CARTESIAN_POINT('',(0.,0.3,0.82));
#7193=CARTESIAN_POINT('',(0.,0.3,1.));
#7194=CARTESIAN_POINT('',(0.,0.3,0.41));
#7195=CARTESIAN_POINT('',(20.,0.3,0.82));
#7196=CARTESIAN_POINT('',(-0.1,0.3,0.82));
#7197=CARTESIAN_POINT('',(20.,0.3,1.));
#7198=CARTESIAN_POINT('',(20.,0.3,0.41));
#7199=CARTESIAN_POINT('',(-0.05,0.3,1.));
#7200=CARTESIAN_POINT('Origin',(-0.1,0.55,0.82));
#7201=CARTESIAN_POINT('',(0.,0.55,0.82));
#7202=CARTESIAN_POINT('',(0.,0.275,0.82));
#7203=CARTESIAN_POINT('',(20.,0.55,0.82));
#7204=CARTESIAN_POINT('',(-0.1,0.55,0.82));
#7205=CARTESIAN_POINT('',(20.,0.275,0.82));
#7206=CARTESIAN_POINT('Origin',(-0.1,0.55,0.67));
#7207=CARTESIAN_POINT('',(0.,0.55,0.67));
#7208=CARTESIAN_POINT('',(0.,0.55,0.335));
#7209=CARTESIAN_POINT('',(20.,0.55,0.67));
#7210=CARTESIAN_POINT('',(-0.1,0.55,0.67));
#7211=CARTESIAN_POINT('',(20.,0.55,0.335));
#7212=CARTESIAN_POINT('Origin',(-0.1,0.3,0.42));
#7213=CARTESIAN_POINT('',(0.,0.3,0.42));
#7214=CARTESIAN_POINT('',(6.93889390390723E-18,0.12,0.24));
#7215=CARTESIAN_POINT('',(20.,0.3,0.42));
#7216=CARTESIAN_POINT('',(-0.1,0.3,0.42));
#7217=CARTESIAN_POINT('',(20.,0.12,0.24));
#7218=CARTESIAN_POINT('Origin',(-0.1,-0.3,0.42));
#7219=CARTESIAN_POINT('',(0.,-0.3,0.42));
#7220=CARTESIAN_POINT('',(0.,-0.15,0.42));
#7221=CARTESIAN_POINT('',(20.,-0.3,0.42));
#7222=CARTESIAN_POINT('',(-0.1,-0.3,0.42));
#7223=CARTESIAN_POINT('',(20.,-0.15,0.42));
#7224=CARTESIAN_POINT('Origin',(-0.1,-0.55,0.67));
#7225=CARTESIAN_POINT('',(0.,-0.55,0.67));
#7226=CARTESIAN_POINT('',(6.93889390390723E-18,-0.245,0.365));
#7227=CARTESIAN_POINT('',(20.,-0.55,0.67));
#7228=CARTESIAN_POINT('',(-0.1,-0.55,0.67));
#7229=CARTESIAN_POINT('',(20.,-0.245,0.365));
#7230=CARTESIAN_POINT('Origin',(-0.1,-0.55,0.82));
#7231=CARTESIAN_POINT('',(0.,-0.55,0.82));
#7232=CARTESIAN_POINT('',(0.,-0.55,0.41));
#7233=CARTESIAN_POINT('',(20.,-0.55,0.82));
#7234=CARTESIAN_POINT('',(-0.1,-0.55,0.82));
#7235=CARTESIAN_POINT('',(20.,-0.55,0.41));
#7236=CARTESIAN_POINT('Origin',(-0.1,-0.3,0.82));
#7237=CARTESIAN_POINT('',(0.,-0.3,0.82));
#7238=CARTESIAN_POINT('',(0.,-0.15,0.82));
#7239=CARTESIAN_POINT('',(20.,-0.3,0.82));
#7240=CARTESIAN_POINT('',(-0.1,-0.3,0.82));
#7241=CARTESIAN_POINT('',(20.,-0.15,0.82));
#7242=CARTESIAN_POINT('Origin',(-0.1,-0.3,1.05));
#7243=CARTESIAN_POINT('',(0.,-0.3,1.));
#7244=CARTESIAN_POINT('',(0.,-0.3,0.525));
#7245=CARTESIAN_POINT('',(20.,-0.3,1.));
#7246=CARTESIAN_POINT('',(-0.05,-0.3,1.));
#7247=CARTESIAN_POINT('',(20.,-0.3,0.525));
#7248=CARTESIAN_POINT('Origin',(-0.1,0.,0.));
#7249=CARTESIAN_POINT('',(0.,-2.57175827820944E-17,0.21));
#7250=CARTESIAN_POINT('Origin',(0.,0.,0.));
#7251=CARTESIAN_POINT('',(20.,2.57175827820944E-17,0.21));
#7252=CARTESIAN_POINT('',(-0.1,-2.57175827820944E-17,0.21));
#7253=CARTESIAN_POINT('Origin',(20.,0.,0.));
#7254=CARTESIAN_POINT('Origin',(0.,1.,-1.));
#7255=CARTESIAN_POINT('',(0.,1.,1.));
#7256=CARTESIAN_POINT('',(0.,1.,-1.));
#7257=CARTESIAN_POINT('',(20.,1.,1.));
#7258=CARTESIAN_POINT('',(0.,1.,1.));
#7259=CARTESIAN_POINT('',(20.,1.,-1.));
#7260=CARTESIAN_POINT('Origin',(0.,1.,-1.));
#7261=CARTESIAN_POINT('',(20.,1.,-1.));
#7262=CARTESIAN_POINT('',(20.,1.,-1.));
#7263=CARTESIAN_POINT('',(0.,1.,-1.));
#7264=CARTESIAN_POINT('',(0.,1.,-1.));
#7265=CARTESIAN_POINT('',(0.,1.,-1.));
#7266=CARTESIAN_POINT('Origin',(0.,-1.,-1.));
#7267=CARTESIAN_POINT('',(0.,-1.,-1.));
#7268=CARTESIAN_POINT('',(20.,-1.,-1.));
#7269=CARTESIAN_POINT('Origin',(0.,-1.,-1.));
#7270=CARTESIAN_POINT('',(20.,-1.,-1.));
#7271=CARTESIAN_POINT('',(20.,-1.,-1.));
#7272=CARTESIAN_POINT('',(0.,-1.,-1.));
#7273=CARTESIAN_POINT('',(0.,-1.,-1.));
#7274=CARTESIAN_POINT('',(0.,-1.,-1.));
#7275=CARTESIAN_POINT('Origin',(0.,-1.,1.));
#7276=CARTESIAN_POINT('',(0.,-1.,1.));
#7277=CARTESIAN_POINT('',(20.,-1.,1.));
#7278=CARTESIAN_POINT('Origin',(0.,-1.,1.));
#7279=CARTESIAN_POINT('',(20.,-1.,1.));
#7280=CARTESIAN_POINT('',(20.,-1.,1.));
#7281=CARTESIAN_POINT('',(0.,-1.,1.));
#7282=CARTESIAN_POINT('',(0.,-1.,1.));
#7283=CARTESIAN_POINT('',(0.,-1.,1.));
#7284=CARTESIAN_POINT('Origin',(0.,1.,1.));
#7285=CARTESIAN_POINT('',(0.,1.,1.));
#7286=CARTESIAN_POINT('',(20.,1.,1.));
#7287=CARTESIAN_POINT('Origin',(0.,1.,1.));
#7288=CARTESIAN_POINT('',(20.,1.,1.));
#7289=CARTESIAN_POINT('',(0.,1.,1.));
#7290=CARTESIAN_POINT('Origin',(20.,0.,0.));
#7291=CARTESIAN_POINT('Origin',(0.,0.,0.));
#7292=CARTESIAN_POINT('',(0.,0.,0.));
#7293=CARTESIAN_POINT('Origin',(0.,0.09,0.));
#7294=CARTESIAN_POINT('',(-0.285,0.1,3.49024337756996E-17));
#7295=CARTESIAN_POINT('Origin',(0.,0.1,0.));
#7296=CARTESIAN_POINT('',(-0.265,0.08,-3.24531401774049E-17));
#7297=CARTESIAN_POINT('',(-0.275,0.09,3.36777869765522E-17));
#7298=CARTESIAN_POINT('Origin',(0.,0.08,0.));
#7299=CARTESIAN_POINT('Origin',(0.,0.,0.));
#7300=CARTESIAN_POINT('',(-0.265,0.,3.24531401774049E-17));
#7301=CARTESIAN_POINT('',(-0.265,0.,3.24531401774049E-17));
#7302=CARTESIAN_POINT('Origin',(0.,0.,0.));
#7303=CARTESIAN_POINT('Origin',(0.,0.1,0.));
#7304=CARTESIAN_POINT('',(-0.5,0.1,6.12323399573677E-17));
#7305=CARTESIAN_POINT('Origin',(0.,0.1,0.));
#7306=CARTESIAN_POINT('Origin',(0.,0.,0.));
#7307=CARTESIAN_POINT('',(-0.5,0.,6.12323399573677E-17));
#7308=CARTESIAN_POINT('',(-0.5,0.,6.12323399573677E-17));
#7309=CARTESIAN_POINT('Origin',(0.,0.,0.));
#7310=CARTESIAN_POINT('Origin',(0.,0.,0.));
#7311=CARTESIAN_POINT('',(0.,0.,0.));
#7312=CARTESIAN_POINT('Origin',(0.115470053837925,-0.5,-0.2));
#7313=CARTESIAN_POINT('',(0.23094010767585,-0.5,0.));
#7314=CARTESIAN_POINT('',(0.115470053837925,-0.5,-0.2));
#7315=CARTESIAN_POINT('',(0.23094010767585,-0.5,0.));
#7316=CARTESIAN_POINT('',(0.115470053837925,-0.8,-0.2));
#7317=CARTESIAN_POINT('',(0.115470053837925,-0.5,-0.2));
#7318=CARTESIAN_POINT('',(0.23094010767585,-0.8,0.));
#7319=CARTESIAN_POINT('',(0.23094010767585,-0.8,0.));
#7320=CARTESIAN_POINT('',(0.23094010767585,-0.5,0.));
#7321=CARTESIAN_POINT('Origin',(-0.115470053837925,-0.5,-0.2));
#7322=CARTESIAN_POINT('',(-0.115470053837925,-0.5,-0.2));
#7323=CARTESIAN_POINT('',(0.115470053837925,-0.5,-0.2));
#7324=CARTESIAN_POINT('',(-0.115470053837925,-0.8,-0.2));
#7325=CARTESIAN_POINT('',(-0.115470053837925,-0.5,-0.2));
#7326=CARTESIAN_POINT('',(0.115470053837925,-0.8,-0.2));
#7327=CARTESIAN_POINT('Origin',(-0.23094010767585,-0.5,-2.77555756156289E-17));
#7328=CARTESIAN_POINT('',(-0.23094010767585,-0.5,-2.82820063659975E-17));
#7329=CARTESIAN_POINT('',(-0.115470053837925,-0.5,-0.2));
#7330=CARTESIAN_POINT('',(-0.23094010767585,-0.8,-2.77555756156289E-17));
#7331=CARTESIAN_POINT('',(-0.23094010767585,-0.5,-2.82820063659975E-17));
#7332=CARTESIAN_POINT('',(-0.115470053837925,-0.8,-0.2));
#7333=CARTESIAN_POINT('Origin',(-0.115470053837925,-0.5,0.2));
#7334=CARTESIAN_POINT('',(-0.115470053837925,-0.5,0.2));
#7335=CARTESIAN_POINT('',(-0.23094010767585,-0.5,-2.82820063659975E-17));
#7336=CARTESIAN_POINT('',(-0.115470053837925,-0.8,0.2));
#7337=CARTESIAN_POINT('',(-0.115470053837925,-0.5,0.2));
#7338=CARTESIAN_POINT('',(-0.23094010767585,-0.8,-2.82820063659975E-17));
#7339=CARTESIAN_POINT('Origin',(0.115470053837925,-0.5,0.2));
#7340=CARTESIAN_POINT('',(0.115470053837925,-0.5,0.2));
#7341=CARTESIAN_POINT('',(-0.115470053837925,-0.5,0.2));
#7342=CARTESIAN_POINT('',(0.115470053837925,-0.8,0.2));
#7343=CARTESIAN_POINT('',(0.115470053837925,-0.5,0.2));
#7344=CARTESIAN_POINT('',(-0.115470053837925,-0.8,0.2));
#7345=CARTESIAN_POINT('Origin',(0.23094010767585,-0.5,0.));
#7346=CARTESIAN_POINT('',(0.115470053837925,-0.5,0.2));
#7347=CARTESIAN_POINT('',(0.115470053837925,-0.8,0.2));
#7348=CARTESIAN_POINT('Origin',(0.,-0.5,0.));
#7349=CARTESIAN_POINT('Origin',(0.,-0.8,0.));
#7350=CARTESIAN_POINT('Origin',(0.,-1.4,0.));
#7351=CARTESIAN_POINT('',(-0.24505,-1.4,3.00099698131059E-17));
#7352=CARTESIAN_POINT('Origin',(0.,-1.4,0.));
#7353=CARTESIAN_POINT('Origin',(0.375,0.5,0.));
#7354=CARTESIAN_POINT('',(-0.375,0.5,-4.59242549680257E-17));
#7355=CARTESIAN_POINT('Origin',(0.,0.5,0.));
#7356=CARTESIAN_POINT('Origin',(0.,0.475,0.));
#7357=CARTESIAN_POINT('',(-0.425,0.45,-5.20474889637625E-17));
#7358=CARTESIAN_POINT('Origin',(0.,0.45,0.));
#7359=CARTESIAN_POINT('',(-0.4,0.475,-4.89858719658941E-17));
#7360=CARTESIAN_POINT('Origin',(0.,0.24,0.));
#7361=CARTESIAN_POINT('',(-0.425,0.0299999999999998,-5.20474889637625E-17));
#7362=CARTESIAN_POINT('Origin',(0.,0.0299999999999998,0.));
#7363=CARTESIAN_POINT('',(-0.425,0.24,-5.20474889637625E-17));
#7364=CARTESIAN_POINT('Origin',(0.,0.0150000000000001,0.));
#7365=CARTESIAN_POINT('',(-0.395,4.85722573273506E-17,-4.83735485663204E-17));
#7366=CARTESIAN_POINT('Origin',(0.,0.,0.));
#7367=CARTESIAN_POINT('',(-0.41,0.0150000000000001,-5.02105187650415E-17));
#7368=CARTESIAN_POINT('Origin',(0.27,0.,0.));
#7369=CARTESIAN_POINT('',(-0.27,0.,-3.30654635769785E-17));
#7370=CARTESIAN_POINT('Origin',(0.,0.,0.));
#7371=CARTESIAN_POINT('Origin',(0.,-0.02,0.));
#7372=CARTESIAN_POINT('',(-0.24505,-0.0498999999999999,3.00099698131059E-17));
#7373=CARTESIAN_POINT('Origin',(0.,-0.0498999999999999,0.));
#7374=CARTESIAN_POINT('',(-0.26,-0.02,-3.18408167778312E-17));
#7375=CARTESIAN_POINT('Origin',(0.,-0.995,0.));
#7376=CARTESIAN_POINT('',(-0.24505,-0.995,-3.00099698131059E-17));
#7377=CARTESIAN_POINT('',(0.,0.,0.));
#7378=CARTESIAN_POINT('Origin',(0.3,0.4,0.));
#7379=CARTESIAN_POINT('',(-0.3,0.4,-3.67394039744206E-17));
#7380=CARTESIAN_POINT('Origin',(0.,0.4,0.));
#7381=CARTESIAN_POINT('Origin',(0.,0.375,0.));
#7382=CARTESIAN_POINT('',(-0.35,0.35,-4.28626379701573E-17));
#7383=CARTESIAN_POINT('Origin',(0.,0.35,0.));
#7384=CARTESIAN_POINT('',(-0.325,0.375,-3.9801020972289E-17));
#7385=CARTESIAN_POINT('Origin',(0.,0.19,0.));
#7386=CARTESIAN_POINT('',(-0.35,0.03,-4.28626379701574E-17));
#7387=CARTESIAN_POINT('Origin',(0.,0.03,0.));
#7388=CARTESIAN_POINT('',(-0.35,0.19,-4.28626379701574E-17));
#7389=CARTESIAN_POINT('Origin',(0.,0.0149999999999999,0.));
#7390=CARTESIAN_POINT('',(-0.32,-3.29597460435593E-17,-3.91886975727153E-17));
#7391=CARTESIAN_POINT('Origin',(0.,0.,0.));
#7392=CARTESIAN_POINT('',(-0.335,0.0149999999999999,-4.10256677714363E-17));
#7393=CARTESIAN_POINT('Origin',(0.22,0.,0.));
#7394=CARTESIAN_POINT('',(-0.22,-6.93889390390723E-18,-2.69422295812418E-17));
#7395=CARTESIAN_POINT('Origin',(0.,0.,0.));
#7396=CARTESIAN_POINT('Origin',(0.,-0.02,0.));
#7397=CARTESIAN_POINT('',(-0.1954,-0.0492,2.39295984553393E-17));
#7398=CARTESIAN_POINT('Origin',(0.,-0.0492,0.));
#7399=CARTESIAN_POINT('',(-0.21,-0.02,-2.57175827820944E-17));
#7400=CARTESIAN_POINT('Origin',(0.,-0.8,0.));
#7401=CARTESIAN_POINT('',(-0.1954,-1.5646,2.39295984553393E-17));
#7402=CARTESIAN_POINT('Origin',(0.,-1.5646,0.));
#7403=CARTESIAN_POINT('',(-0.1954,-0.8,-2.39295984553393E-17));
#7404=CARTESIAN_POINT('Origin',(0.,-1.58,0.));
#7405=CARTESIAN_POINT('',(-0.16,-1.6,-1.95943487863577E-17));
#7406=CARTESIAN_POINT('Origin',(0.,-1.6,0.));
#7407=CARTESIAN_POINT('',(-0.18,-1.58,-2.20436423846524E-17));
#7408=CARTESIAN_POINT('Origin',(0.,-1.6,0.));
#7409=CARTESIAN_POINT('Origin',(0.0866025403784439,-0.4,-0.15));
#7410=CARTESIAN_POINT('',(0.173205080756888,-0.4,0.));
#7411=CARTESIAN_POINT('',(0.0866025403784439,-0.4,-0.15));
#7412=CARTESIAN_POINT('',(0.173205080756888,-0.4,0.));
#7413=CARTESIAN_POINT('',(0.0866025403784439,-0.64,-0.15));
#7414=CARTESIAN_POINT('',(0.0866025403784439,-0.4,-0.15));
#7415=CARTESIAN_POINT('',(0.173205080756888,-0.64,0.));
#7416=CARTESIAN_POINT('',(0.173205080756888,-0.64,0.));
#7417=CARTESIAN_POINT('',(0.173205080756888,-0.4,0.));
#7418=CARTESIAN_POINT('Origin',(-0.0866025403784438,-0.4,-0.15));
#7419=CARTESIAN_POINT('',(-0.0866025403784438,-0.4,-0.15));
#7420=CARTESIAN_POINT('',(0.0866025403784439,-0.4,-0.15));
#7421=CARTESIAN_POINT('',(-0.0866025403784438,-0.64,-0.15));
#7422=CARTESIAN_POINT('',(-0.0866025403784438,-0.4,-0.15));
#7423=CARTESIAN_POINT('',(0.0866025403784439,-0.64,-0.15));
#7424=CARTESIAN_POINT('Origin',(-0.173205080756888,-0.4,-2.77555756156289E-17));
#7425=CARTESIAN_POINT('',(-0.173205080756888,-0.4,-2.12115047744981E-17));
#7426=CARTESIAN_POINT('',(-0.0866025403784438,-0.4,-0.15));
#7427=CARTESIAN_POINT('',(-0.173205080756888,-0.64,-2.77555756156289E-17));
#7428=CARTESIAN_POINT('',(-0.173205080756888,-0.4,-2.12115047744981E-17));
#7429=CARTESIAN_POINT('',(-0.0866025403784438,-0.64,-0.15));
#7430=CARTESIAN_POINT('Origin',(-0.0866025403784439,-0.4,0.15));
#7431=CARTESIAN_POINT('',(-0.0866025403784439,-0.4,0.15));
#7432=CARTESIAN_POINT('',(-0.173205080756888,-0.4,-2.12115047744981E-17));
#7433=CARTESIAN_POINT('',(-0.0866025403784439,-0.64,0.15));
#7434=CARTESIAN_POINT('',(-0.0866025403784439,-0.4,0.15));
#7435=CARTESIAN_POINT('',(-0.173205080756888,-0.64,-2.12115047744981E-17));
#7436=CARTESIAN_POINT('Origin',(0.0866025403784439,-0.4,0.15));
#7437=CARTESIAN_POINT('',(0.0866025403784439,-0.4,0.15));
#7438=CARTESIAN_POINT('',(-0.0866025403784439,-0.4,0.15));
#7439=CARTESIAN_POINT('',(0.0866025403784439,-0.64,0.15));
#7440=CARTESIAN_POINT('',(0.0866025403784439,-0.4,0.15));
#7441=CARTESIAN_POINT('',(-0.0866025403784439,-0.64,0.15));
#7442=CARTESIAN_POINT('Origin',(0.173205080756888,-0.4,0.));
#7443=CARTESIAN_POINT('',(0.0866025403784439,-0.4,0.15));
#7444=CARTESIAN_POINT('',(0.0866025403784439,-0.64,0.15));
#7445=CARTESIAN_POINT('Origin',(0.,-0.4,-2.77555756156289E-17));
#7446=CARTESIAN_POINT('Origin',(0.,-0.64,-2.77555756156289E-17));
#7447=CARTESIAN_POINT('',(0.,0.,0.));
#7448=CARTESIAN_POINT('Origin',(0.,-0.4,0.));
#7449=CARTESIAN_POINT('',(1.01036297108185,-0.4,0.));
#7450=CARTESIAN_POINT('',(0.505181485540923,-0.4,0.875));
#7451=CARTESIAN_POINT('',(0.505181485540923,-0.4,0.875));
#7452=CARTESIAN_POINT('',(-0.505181485540923,-0.4,0.875));
#7453=CARTESIAN_POINT('',(-0.505181485540923,-0.4,0.875));
#7454=CARTESIAN_POINT('',(-1.01036297108185,-0.4,-1.23733777851239E-16));
#7455=CARTESIAN_POINT('',(-1.01036297108185,-0.4,-1.23733777851239E-16));
#7456=CARTESIAN_POINT('',(-0.505181485540922,-0.4,-0.875));
#7457=CARTESIAN_POINT('',(-0.505181485540922,-0.4,-0.875));
#7458=CARTESIAN_POINT('',(0.505181485540923,-0.4,-0.875));
#7459=CARTESIAN_POINT('',(0.505181485540923,-0.4,-0.875));
#7460=CARTESIAN_POINT('',(1.01036297108185,-0.4,0.));
#7461=CARTESIAN_POINT('',(-0.685,-0.4,-8.38883057415937E-17));
#7462=CARTESIAN_POINT('Origin',(0.,-0.4,0.));
#7463=CARTESIAN_POINT('Origin',(0.,0.4,0.));
#7464=CARTESIAN_POINT('',(0.505181485540923,0.4,0.875));
#7465=CARTESIAN_POINT('',(1.01036297108185,0.4,0.));
#7466=CARTESIAN_POINT('',(0.505181485540923,0.4,0.875));
#7467=CARTESIAN_POINT('',(0.505181485540923,0.4,-0.875));
#7468=CARTESIAN_POINT('',(1.01036297108185,0.4,0.));
#7469=CARTESIAN_POINT('',(-0.505181485540922,0.4,-0.875));
#7470=CARTESIAN_POINT('',(0.505181485540923,0.4,-0.875));
#7471=CARTESIAN_POINT('',(-1.01036297108185,0.4,-1.23733777851239E-16));
#7472=CARTESIAN_POINT('',(-0.505181485540922,0.4,-0.875));
#7473=CARTESIAN_POINT('',(-0.505181485540923,0.4,0.875));
#7474=CARTESIAN_POINT('',(-1.01036297108185,0.4,-1.23733777851239E-16));
#7475=CARTESIAN_POINT('',(-0.505181485540923,0.4,0.875));
#7476=CARTESIAN_POINT('',(-0.685,0.4,8.38883057415937E-17));
#7477=CARTESIAN_POINT('Origin',(0.,0.4,0.));
#7478=CARTESIAN_POINT('Origin',(-0.505181485540923,0.,0.875));
#7479=CARTESIAN_POINT('',(0.505181485540923,0.,0.875));
#7480=CARTESIAN_POINT('',(-0.505181485540923,0.,0.875));
#7481=CARTESIAN_POINT('Origin',(-1.01036297108185,0.,-1.23733777851239E-16));
#7482=CARTESIAN_POINT('',(-1.01036297108185,0.,-1.23733777851239E-16));
#7483=CARTESIAN_POINT('Origin',(-0.505181485540922,0.,-0.875));
#7484=CARTESIAN_POINT('',(-0.505181485540922,0.,-0.875));
#7485=CARTESIAN_POINT('Origin',(0.505181485540923,0.,-0.875));
#7486=CARTESIAN_POINT('',(0.505181485540923,0.,-0.875));
#7487=CARTESIAN_POINT('Origin',(1.01036297108185,0.,0.));
#7488=CARTESIAN_POINT('',(1.01036297108185,0.,0.));
#7489=CARTESIAN_POINT('Origin',(0.505181485540923,0.,0.875));
#7490=CARTESIAN_POINT('Origin',(0.,0.,0.));
#7491=CARTESIAN_POINT('',(-0.685,1.82,-8.38883057415937E-17));
#7492=CARTESIAN_POINT('',(-0.685,0.,-8.38883057415937E-17));
#7493=CARTESIAN_POINT('Origin',(0.,1.82,0.));
#7494=CARTESIAN_POINT('Origin',(0.605,1.9,0.));
#7495=CARTESIAN_POINT('',(-0.605,1.9,-7.40911313484149E-17));
#7496=CARTESIAN_POINT('Origin',(0.,1.9,0.));
#7497=CARTESIAN_POINT('',(-0.46,1.9,-5.63337527607782E-17));
#7498=CARTESIAN_POINT('Origin',(0.,1.9,0.));
#7499=CARTESIAN_POINT('Origin',(0.,1.86,0.));
#7500=CARTESIAN_POINT('',(-0.645,1.86,-7.89897185450043E-17));
#7501=CARTESIAN_POINT('Origin',(0.,0.,0.));
#7502=CARTESIAN_POINT('',(-0.685,-1.82,-8.38883057415937E-17));
#7503=CARTESIAN_POINT('Origin',(0.,-1.82,0.));
#7504=CARTESIAN_POINT('',(-0.685,0.,-8.38883057415937E-17));
#7505=CARTESIAN_POINT('Origin',(0.,-1.86,0.));
#7506=CARTESIAN_POINT('',(-0.605,-1.9,-7.40911313484149E-17));
#7507=CARTESIAN_POINT('Origin',(0.,-1.9,0.));
#7508=CARTESIAN_POINT('',(-0.645,-1.86,-7.89897185450043E-17));
#7509=CARTESIAN_POINT('Origin',(0.46,-1.9,0.));
#7510=CARTESIAN_POINT('',(-0.46,-1.9,-5.63337527607782E-17));
#7511=CARTESIAN_POINT('Origin',(0.,-1.9,0.));
#7512=CARTESIAN_POINT('Origin',(0.,0.,0.));
#7513=CARTESIAN_POINT('',(-0.46,0.,-5.63337527607782E-17));
#7514=CARTESIAN_POINT('',(0.,0.,0.));
#7515=CARTESIAN_POINT('',(0.,0.,0.));
#7516=CARTESIAN_POINT('',(0.,0.,0.));
#7517=CARTESIAN_POINT('',(0.,0.,0.));
#7518=CARTESIAN_POINT('',(0.,0.,0.));
#7519=CARTESIAN_POINT('',(0.,0.,0.));
#7520=CARTESIAN_POINT('',(0.,0.,0.));
#7521=CARTESIAN_POINT('',(0.,0.,0.));
#7522=CARTESIAN_POINT('',(0.,0.,0.));
#7523=CARTESIAN_POINT('',(0.,3.,0.8));
#7524=CARTESIAN_POINT('',(0.,3.,0.));
#7525=CARTESIAN_POINT('',(0.,3.,-0.1));
#7526=CARTESIAN_POINT('',(0.,3.,21.5));
#7527=CARTESIAN_POINT('',(0.,3.,21.6));
#7528=CARTESIAN_POINT('',(-4.3,1.,22.3));
#7529=CARTESIAN_POINT('',(4.3,1.,22.3));
#7530=CARTESIAN_POINT('',(5.5,0.,23.));
#7531=CARTESIAN_POINT('',(0.,0.,0.));
#7532=CARTESIAN_POINT('',(0.,0.,0.));
#7533=CARTESIAN_POINT('Origin',(-3.,-3.6,23.));
#7534=CARTESIAN_POINT('',(-3.515,-3.5,23.));
#7535=CARTESIAN_POINT('Origin',(-3.,-3.5,23.));
#7536=CARTESIAN_POINT('',(-3.515,-2.85,23.));
#7537=CARTESIAN_POINT('',(-3.515,-3.6,23.));
#7538=CARTESIAN_POINT('Origin',(-3.,-2.85,23.));
#7539=CARTESIAN_POINT('Origin',(-3.,-2.85,23.));
#7540=CARTESIAN_POINT('',(-3.2,-2.85,23.));
#7541=CARTESIAN_POINT('Origin',(-3.,-2.85,23.));
#7542=CARTESIAN_POINT('Origin',(-3.,-3.6,23.));
#7543=CARTESIAN_POINT('',(-3.2,-1.02020410288673,23.));
#7544=CARTESIAN_POINT('',(-3.2,-3.6,23.));
#7545=CARTESIAN_POINT('Origin',(-3.,-1.02020410288673,23.));
#7546=CARTESIAN_POINT('Origin',(-3.,-3.5,23.));
#7547=CARTESIAN_POINT('',(-3.6,-2.8,23.));
#7548=CARTESIAN_POINT('Origin',(-3.,-2.8,23.));
#7549=CARTESIAN_POINT('',(-3.6,-3.5,23.));
#7550=CARTESIAN_POINT('',(-3.6,-3.5,23.));
#7551=CARTESIAN_POINT('Origin',(-3.,-3.5,23.));
#7552=CARTESIAN_POINT('Origin',(-3.,-3.5,23.));
#7553=CARTESIAN_POINT('Origin',(-3.,-2.,23.));
#7554=CARTESIAN_POINT('',(-3.,-2.,24.));
#7555=CARTESIAN_POINT('',(-3.,-2.,22.));
#7556=CARTESIAN_POINT('Origin',(-3.,-2.,23.));
#7557=CARTESIAN_POINT('',(0.,0.,0.));
#7558=CARTESIAN_POINT('Origin',(-3.,-7.2,23.));
#7559=CARTESIAN_POINT('',(-3.2,-4.2,23.));
#7560=CARTESIAN_POINT('Origin',(-3.,-4.2,23.));
#7561=CARTESIAN_POINT('',(-3.2,-7.2,23.));
#7562=CARTESIAN_POINT('',(-3.2,-7.2,23.));
#7563=CARTESIAN_POINT('Origin',(-3.,-7.2,23.));
#7564=CARTESIAN_POINT('Origin',(-3.,-7.2,23.));
#7565=CARTESIAN_POINT('',(-3.3,-4.2,23.));
#7566=CARTESIAN_POINT('Origin',(-3.,-4.2,23.));
#7567=CARTESIAN_POINT('',(-3.3,-7.2,23.));
#7568=CARTESIAN_POINT('',(-3.3,-7.2,23.));
#7569=CARTESIAN_POINT('Origin',(-3.,-7.2,23.));
#7570=CARTESIAN_POINT('Origin',(-3.,-4.2,23.));
#7571=CARTESIAN_POINT('Origin',(-3.,-7.2,23.));
#7572=CARTESIAN_POINT('',(0.,0.,0.));
#7573=CARTESIAN_POINT('Origin',(-3.,-7.2,23.));
#7574=CARTESIAN_POINT('',(-3.3,-7.2,23.));
#7575=CARTESIAN_POINT('Origin',(-3.,-7.2,23.));
#7576=CARTESIAN_POINT('',(-3.3,-6.9,23.));
#7577=CARTESIAN_POINT('',(-3.3,-7.2,23.));
#7578=CARTESIAN_POINT('Origin',(-3.,-6.9,23.));
#7579=CARTESIAN_POINT('Origin',(-3.,-7.2,23.));
#7580=CARTESIAN_POINT('',(-3.075,-7.2,23.));
#7581=CARTESIAN_POINT('Origin',(-3.,-7.2,23.));
#7582=CARTESIAN_POINT('Origin',(-3.,-7.7,23.));
#7583=CARTESIAN_POINT('',(-3.075,-7.7,23.));
#7584=CARTESIAN_POINT('',(-3.075,-7.7,23.));
#7585=CARTESIAN_POINT('Origin',(-3.,-7.7,23.));
#7586=CARTESIAN_POINT('Origin',(-3.,-7.7,23.));
#7587=CARTESIAN_POINT('',(-3.4,-6.9,23.));
#7588=CARTESIAN_POINT('Origin',(-3.,-6.9,23.));
#7589=CARTESIAN_POINT('',(-3.4,-7.7,23.));
#7590=CARTESIAN_POINT('',(-3.4,-7.7,23.));
#7591=CARTESIAN_POINT('Origin',(-3.,-7.7,23.));
#7592=CARTESIAN_POINT('Origin',(-3.,-6.9,23.));
#7593=CARTESIAN_POINT('Origin',(-3.,-7.7,23.));
#7594=CARTESIAN_POINT('',(0.,0.,0.));
#7595=CARTESIAN_POINT('',(0.,0.,0.));
#7596=CARTESIAN_POINT('Origin',(0.,-3.6,23.));
#7597=CARTESIAN_POINT('',(-0.515,-3.5,23.));
#7598=CARTESIAN_POINT('Origin',(0.,-3.5,23.));
#7599=CARTESIAN_POINT('',(-0.515,-2.85,23.));
#7600=CARTESIAN_POINT('',(-0.515,-3.6,23.));
#7601=CARTESIAN_POINT('Origin',(0.,-2.85,23.));
#7602=CARTESIAN_POINT('Origin',(0.,-2.85,23.));
#7603=CARTESIAN_POINT('',(-0.2,-2.85,23.));
#7604=CARTESIAN_POINT('Origin',(0.,-2.85,23.));
#7605=CARTESIAN_POINT('Origin',(0.,-3.6,23.));
#7606=CARTESIAN_POINT('',(-0.2,-1.02020410288673,23.));
#7607=CARTESIAN_POINT('',(-0.2,-3.6,23.));
#7608=CARTESIAN_POINT('Origin',(0.,-1.02020410288673,23.));
#7609=CARTESIAN_POINT('Origin',(0.,-3.5,23.));
#7610=CARTESIAN_POINT('',(-0.6,-2.8,23.));
#7611=CARTESIAN_POINT('Origin',(0.,-2.8,23.));
#7612=CARTESIAN_POINT('',(-0.6,-3.5,23.));
#7613=CARTESIAN_POINT('',(-0.6,-3.5,23.));
#7614=CARTESIAN_POINT('Origin',(0.,-3.5,23.));
#7615=CARTESIAN_POINT('Origin',(0.,-3.5,23.));
#7616=CARTESIAN_POINT('Origin',(0.,-2.,23.));
#7617=CARTESIAN_POINT('',(-6.12323399573677E-17,-2.,24.));
#7618=CARTESIAN_POINT('',(-6.12323399573677E-17,-2.,22.));
#7619=CARTESIAN_POINT('Origin',(0.,-2.,23.));
#7620=CARTESIAN_POINT('',(0.,0.,0.));
#7621=CARTESIAN_POINT('Origin',(0.,-7.2,23.));
#7622=CARTESIAN_POINT('',(-0.2,-4.2,23.));
#7623=CARTESIAN_POINT('Origin',(0.,-4.2,23.));
#7624=CARTESIAN_POINT('',(-0.2,-7.2,23.));
#7625=CARTESIAN_POINT('',(-0.2,-7.2,23.));
#7626=CARTESIAN_POINT('Origin',(0.,-7.2,23.));
#7627=CARTESIAN_POINT('Origin',(0.,-7.2,23.));
#7628=CARTESIAN_POINT('',(-0.3,-4.2,23.));
#7629=CARTESIAN_POINT('Origin',(0.,-4.2,23.));
#7630=CARTESIAN_POINT('',(-0.3,-7.2,23.));
#7631=CARTESIAN_POINT('',(-0.3,-7.2,23.));
#7632=CARTESIAN_POINT('Origin',(0.,-7.2,23.));
#7633=CARTESIAN_POINT('Origin',(0.,-4.2,23.));
#7634=CARTESIAN_POINT('Origin',(0.,-7.2,23.));
#7635=CARTESIAN_POINT('',(0.,0.,0.));
#7636=CARTESIAN_POINT('Origin',(0.,-7.2,23.));
#7637=CARTESIAN_POINT('',(-0.3,-7.2,23.));
#7638=CARTESIAN_POINT('Origin',(0.,-7.2,23.));
#7639=CARTESIAN_POINT('',(-0.3,-6.9,23.));
#7640=CARTESIAN_POINT('',(-0.3,-7.2,23.));
#7641=CARTESIAN_POINT('Origin',(0.,-6.9,23.));
#7642=CARTESIAN_POINT('Origin',(0.,-7.2,23.));
#7643=CARTESIAN_POINT('',(-0.075,-7.2,23.));
#7644=CARTESIAN_POINT('Origin',(0.,-7.2,23.));
#7645=CARTESIAN_POINT('Origin',(0.,-7.7,23.));
#7646=CARTESIAN_POINT('',(-0.075,-7.7,23.));
#7647=CARTESIAN_POINT('',(-0.075,-7.7,23.));
#7648=CARTESIAN_POINT('Origin',(0.,-7.7,23.));
#7649=CARTESIAN_POINT('Origin',(0.,-7.7,23.));
#7650=CARTESIAN_POINT('',(-0.4,-6.9,23.));
#7651=CARTESIAN_POINT('Origin',(0.,-6.9,23.));
#7652=CARTESIAN_POINT('',(-0.4,-7.7,23.));
#7653=CARTESIAN_POINT('',(-0.4,-7.7,23.));
#7654=CARTESIAN_POINT('Origin',(0.,-7.7,23.));
#7655=CARTESIAN_POINT('Origin',(0.,-6.9,23.));
#7656=CARTESIAN_POINT('Origin',(0.,-7.7,23.));
#7657=CARTESIAN_POINT('',(0.,0.,0.));
#7658=CARTESIAN_POINT('',(0.,0.,0.));
#7659=CARTESIAN_POINT('Origin',(3.,-3.6,23.));
#7660=CARTESIAN_POINT('',(2.485,-3.5,23.));
#7661=CARTESIAN_POINT('Origin',(3.,-3.5,23.));
#7662=CARTESIAN_POINT('',(2.485,-2.85,23.));
#7663=CARTESIAN_POINT('',(2.485,-3.6,23.));
#7664=CARTESIAN_POINT('Origin',(3.,-2.85,23.));
#7665=CARTESIAN_POINT('Origin',(3.,-2.85,23.));
#7666=CARTESIAN_POINT('',(2.8,-2.85,23.));
#7667=CARTESIAN_POINT('Origin',(3.,-2.85,23.));
#7668=CARTESIAN_POINT('Origin',(3.,-3.6,23.));
#7669=CARTESIAN_POINT('',(2.8,-1.02020410288673,23.));
#7670=CARTESIAN_POINT('',(2.8,-3.6,23.));
#7671=CARTESIAN_POINT('Origin',(3.,-1.02020410288673,23.));
#7672=CARTESIAN_POINT('Origin',(3.,-3.5,23.));
#7673=CARTESIAN_POINT('',(2.4,-2.8,23.));
#7674=CARTESIAN_POINT('Origin',(3.,-2.8,23.));
#7675=CARTESIAN_POINT('',(2.4,-3.5,23.));
#7676=CARTESIAN_POINT('',(2.4,-3.5,23.));
#7677=CARTESIAN_POINT('Origin',(3.,-3.5,23.));
#7678=CARTESIAN_POINT('Origin',(3.,-3.5,23.));
#7679=CARTESIAN_POINT('Origin',(3.,-2.,23.));
#7680=CARTESIAN_POINT('',(3.,-2.,24.));
#7681=CARTESIAN_POINT('',(3.,-2.,22.));
#7682=CARTESIAN_POINT('Origin',(3.,-2.,23.));
#7683=CARTESIAN_POINT('',(0.,0.,0.));
#7684=CARTESIAN_POINT('Origin',(3.,-7.2,23.));
#7685=CARTESIAN_POINT('',(2.8,-4.2,23.));
#7686=CARTESIAN_POINT('Origin',(3.,-4.2,23.));
#7687=CARTESIAN_POINT('',(2.8,-7.2,23.));
#7688=CARTESIAN_POINT('',(2.8,-7.2,23.));
#7689=CARTESIAN_POINT('Origin',(3.,-7.2,23.));
#7690=CARTESIAN_POINT('Origin',(3.,-7.2,23.));
#7691=CARTESIAN_POINT('',(2.7,-4.2,23.));
#7692=CARTESIAN_POINT('Origin',(3.,-4.2,23.));
#7693=CARTESIAN_POINT('',(2.7,-7.2,23.));
#7694=CARTESIAN_POINT('',(2.7,-7.2,23.));
#7695=CARTESIAN_POINT('Origin',(3.,-7.2,23.));
#7696=CARTESIAN_POINT('Origin',(3.,-4.2,23.));
#7697=CARTESIAN_POINT('Origin',(3.,-7.2,23.));
#7698=CARTESIAN_POINT('',(0.,0.,0.));
#7699=CARTESIAN_POINT('Origin',(3.,-7.2,23.));
#7700=CARTESIAN_POINT('',(2.7,-7.2,23.));
#7701=CARTESIAN_POINT('Origin',(3.,-7.2,23.));
#7702=CARTESIAN_POINT('',(2.7,-6.9,23.));
#7703=CARTESIAN_POINT('',(2.7,-7.2,23.));
#7704=CARTESIAN_POINT('Origin',(3.,-6.9,23.));
#7705=CARTESIAN_POINT('Origin',(3.,-7.2,23.));
#7706=CARTESIAN_POINT('',(2.925,-7.2,23.));
#7707=CARTESIAN_POINT('Origin',(3.,-7.2,23.));
#7708=CARTESIAN_POINT('Origin',(3.,-7.7,23.));
#7709=CARTESIAN_POINT('',(2.925,-7.7,23.));
#7710=CARTESIAN_POINT('',(2.925,-7.7,23.));
#7711=CARTESIAN_POINT('Origin',(3.,-7.7,23.));
#7712=CARTESIAN_POINT('Origin',(3.,-7.7,23.));
#7713=CARTESIAN_POINT('',(2.6,-6.9,23.));
#7714=CARTESIAN_POINT('Origin',(3.,-6.9,23.));
#7715=CARTESIAN_POINT('',(2.6,-7.7,23.));
#7716=CARTESIAN_POINT('',(2.6,-7.7,23.));
#7717=CARTESIAN_POINT('Origin',(3.,-7.7,23.));
#7718=CARTESIAN_POINT('Origin',(3.,-6.9,23.));
#7719=CARTESIAN_POINT('Origin',(3.,-7.7,23.));
#7720=CARTESIAN_POINT('',(0.,0.,0.));
#7721=CARTESIAN_POINT('',(0.,0.,0.));
#7722=CARTESIAN_POINT('Origin',(0.,0.6,0.));
#7723=CARTESIAN_POINT('',(-0.43,0.6,5.26598123633362E-17));
#7724=CARTESIAN_POINT('Origin',(0.,0.6,0.));
#7725=CARTESIAN_POINT('',(-0.43,0.7,-5.26598123633362E-17));
#7726=CARTESIAN_POINT('',(-0.43,0.6,5.26598123633362E-17));
#7727=CARTESIAN_POINT('Origin',(0.,0.7,0.));
#7728=CARTESIAN_POINT('Origin',(0.,0.6,0.));
#7729=CARTESIAN_POINT('',(-0.2,0.6,2.44929359829471E-17));
#7730=CARTESIAN_POINT('Origin',(0.,0.6,0.));
#7731=CARTESIAN_POINT('Origin',(0.,0.5,-1.11022302462516E-16));
#7732=CARTESIAN_POINT('',(0.346410161513776,0.5,0.6));
#7733=CARTESIAN_POINT('',(0.692820323027551,0.5,0.));
#7734=CARTESIAN_POINT('',(0.346410161513776,0.5,0.6));
#7735=CARTESIAN_POINT('',(0.346410161513776,0.5,-0.6));
#7736=CARTESIAN_POINT('',(0.692820323027551,0.5,0.));
#7737=CARTESIAN_POINT('',(-0.346410161513775,0.5,-0.6));
#7738=CARTESIAN_POINT('',(0.346410161513776,0.5,-0.6));
#7739=CARTESIAN_POINT('',(-0.692820323027551,0.5,-8.48460190979926E-17));
#7740=CARTESIAN_POINT('',(-0.346410161513775,0.5,-0.6));
#7741=CARTESIAN_POINT('',(-0.346410161513776,0.5,0.6));
#7742=CARTESIAN_POINT('',(-0.692820323027551,0.5,-8.48460190979926E-17));
#7743=CARTESIAN_POINT('',(-0.346410161513776,0.5,0.6));
#7744=CARTESIAN_POINT('',(-0.525,0.5,-6.4293956955236E-17));
#7745=CARTESIAN_POINT('Origin',(0.,0.5,0.));
#7746=CARTESIAN_POINT('Origin',(0.,0.,-1.11022302462516E-16));
#7747=CARTESIAN_POINT('',(0.346410161513776,0.,0.6));
#7748=CARTESIAN_POINT('',(0.692820323027551,0.,0.));
#7749=CARTESIAN_POINT('',(0.346410161513776,0.,0.6));
#7750=CARTESIAN_POINT('',(-0.346410161513776,0.,0.6));
#7751=CARTESIAN_POINT('',(-0.346410161513776,0.,0.6));
#7752=CARTESIAN_POINT('',(-0.692820323027551,0.,-8.48460190979926E-17));
#7753=CARTESIAN_POINT('',(-0.692820323027551,0.,-8.48460190979926E-17));
#7754=CARTESIAN_POINT('',(-0.346410161513775,0.,-0.6));
#7755=CARTESIAN_POINT('',(-0.346410161513775,0.,-0.6));
#7756=CARTESIAN_POINT('',(0.346410161513776,0.,-0.6));
#7757=CARTESIAN_POINT('',(0.346410161513776,0.,-0.6));
#7758=CARTESIAN_POINT('',(0.692820323027551,0.,0.));
#7759=CARTESIAN_POINT('',(-0.515,0.,-6.30693101560887E-17));
#7760=CARTESIAN_POINT('Origin',(0.,0.,0.));
#7761=CARTESIAN_POINT('Origin',(-0.346410161513776,0.,0.6));
#7762=CARTESIAN_POINT('',(0.346410161513776,0.,0.6));
#7763=CARTESIAN_POINT('',(-0.346410161513776,0.,0.6));
#7764=CARTESIAN_POINT('Origin',(-0.692820323027551,0.,-8.48460190979926E-17));
#7765=CARTESIAN_POINT('',(-0.692820323027551,0.,-8.48460190979926E-17));
#7766=CARTESIAN_POINT('Origin',(-0.346410161513775,0.,-0.6));
#7767=CARTESIAN_POINT('',(-0.346410161513775,0.,-0.6));
#7768=CARTESIAN_POINT('Origin',(0.346410161513776,0.,-0.6));
#7769=CARTESIAN_POINT('',(0.346410161513776,0.,-0.6));
#7770=CARTESIAN_POINT('Origin',(0.692820323027551,0.,0.));
#7771=CARTESIAN_POINT('',(0.692820323027551,0.,0.));
#7772=CARTESIAN_POINT('Origin',(0.346410161513776,0.,0.6));
#7773=CARTESIAN_POINT('Origin',(0.46,0.7,0.));
#7774=CARTESIAN_POINT('',(-0.46,0.7,-5.63337527607782E-17));
#7775=CARTESIAN_POINT('Origin',(0.,0.7,0.));
#7776=CARTESIAN_POINT('Origin',(0.,1.2,0.));
#7777=CARTESIAN_POINT('',(-0.46,1.7,-5.63337527607782E-17));
#7778=CARTESIAN_POINT('',(-0.46,1.2,-5.63337527607782E-17));
#7779=CARTESIAN_POINT('Origin',(0.,1.7,0.));
#7780=CARTESIAN_POINT('Origin',(0.525,1.7,0.));
#7781=CARTESIAN_POINT('',(-0.525,1.7,-6.4293956955236E-17));
#7782=CARTESIAN_POINT('Origin',(0.,1.7,0.));
#7783=CARTESIAN_POINT('Origin',(0.,1.1,0.));
#7784=CARTESIAN_POINT('',(-0.525,1.1,-6.4293956955236E-17));
#7785=CARTESIAN_POINT('Origin',(0.,-0.325,0.));
#7786=CARTESIAN_POINT('',(-0.515,-0.65,-6.30693101560887E-17));
#7787=CARTESIAN_POINT('Origin',(0.,-0.65,0.));
#7788=CARTESIAN_POINT('',(-0.515,-0.325,-6.30693101560887E-17));
#7789=CARTESIAN_POINT('Origin',(0.2,-0.65,0.));
#7790=CARTESIAN_POINT('',(-0.2,-0.65,-2.44929359829471E-17));
#7791=CARTESIAN_POINT('Origin',(0.,-0.65,0.));
#7792=CARTESIAN_POINT('Origin',(0.,0.0249999999999999,0.));
#7793=CARTESIAN_POINT('',(-0.2,0.0249999999999999,-2.44929359829471E-17));
#7794=CARTESIAN_POINT('',(0.,0.,0.));
#7795=CARTESIAN_POINT('Origin',(0.475,1.95,0.));
#7796=CARTESIAN_POINT('',(-0.475,1.95,-5.81707229594993E-17));
#7797=CARTESIAN_POINT('Origin',(0.,1.95,0.));
#7798=CARTESIAN_POINT('',(-0.31,1.95,-3.7964050773568E-17));
#7799=CARTESIAN_POINT('Origin',(0.,1.95,0.));
#7800=CARTESIAN_POINT('Origin',(0.,1.825,0.));
#7801=CARTESIAN_POINT('',(-0.475,1.7,-5.81707229594993E-17));
#7802=CARTESIAN_POINT('Origin',(0.,1.7,0.));
#7803=CARTESIAN_POINT('',(-0.475,1.825,-5.81707229594993E-17));
#7804=CARTESIAN_POINT('Origin',(0.355,1.7,0.));
#7805=CARTESIAN_POINT('',(-0.355,1.7,-4.3474961369731E-17));
#7806=CARTESIAN_POINT('Origin',(0.,1.7,0.));
#7807=CARTESIAN_POINT('Origin',(0.,1.55,0.));
#7808=CARTESIAN_POINT('',(-0.355,1.4,-4.3474961369731E-17));
#7809=CARTESIAN_POINT('Origin',(0.,1.4,0.));
#7810=CARTESIAN_POINT('',(-0.355,1.55,-4.3474961369731E-17));
#7811=CARTESIAN_POINT('Origin',(0.31,1.4,0.));
#7812=CARTESIAN_POINT('',(-0.31,1.4,-3.7964050773568E-17));
#7813=CARTESIAN_POINT('Origin',(0.,1.4,0.));
#7814=CARTESIAN_POINT('Origin',(0.,1.675,0.));
#7815=CARTESIAN_POINT('',(-0.31,1.675,-3.7964050773568E-17));
#7816=CARTESIAN_POINT('',(0.,0.,0.));
#7817=CARTESIAN_POINT('',(0.,0.,0.));
#7818=CARTESIAN_POINT('',(0.,0.,0.));
#7819=CARTESIAN_POINT('',(0.,0.,0.));
#7820=CARTESIAN_POINT('',(0.,0.,0.));
#7821=CARTESIAN_POINT('',(-3.,-3.5,23.));
#7822=CARTESIAN_POINT('',(0.,0.,0.));
#7823=CARTESIAN_POINT('',(0.,0.,0.));
#7824=CARTESIAN_POINT('',(0.,0.,0.));
#7825=CARTESIAN_POINT('',(0.,-3.5,23.));
#7826=CARTESIAN_POINT('',(0.,0.,0.));
#7827=CARTESIAN_POINT('',(0.,0.,0.));
#7828=CARTESIAN_POINT('',(0.,0.,0.));
#7829=CARTESIAN_POINT('',(3.,-3.5,23.));
#7830=CARTESIAN_POINT('',(0.,0.,0.));
#7831=CARTESIAN_POINT('',(0.,0.,0.));
#7832=CARTESIAN_POINT('',(0.,0.,0.));
#7833=CARTESIAN_POINT('',(0.,0.,0.));
#7834=UNCERTAINTY_MEASURE_WITH_UNIT(LENGTH_MEASURE(0.001),#7898,
'DISTANCE_ACCURACY_VALUE',
'Maximum model space distance between geometric entities at asserted c
onnectivities');
#7835=UNCERTAINTY_MEASURE_WITH_UNIT(LENGTH_MEASURE(0.001),#7898,
'DISTANCE_ACCURACY_VALUE',
'Maximum model space distance between geometric entities at asserted c
onnectivities');
#7836=UNCERTAINTY_MEASURE_WITH_UNIT(LENGTH_MEASURE(0.001),#7898,
'DISTANCE_ACCURACY_VALUE',
'Maximum model space distance between geometric entities at asserted c
onnectivities');
#7837=UNCERTAINTY_MEASURE_WITH_UNIT(LENGTH_MEASURE(0.001),#7898,
'DISTANCE_ACCURACY_VALUE',
'Maximum model space distance between geometric entities at asserted c
onnectivities');
#7838=UNCERTAINTY_MEASURE_WITH_UNIT(LENGTH_MEASURE(0.001),#7898,
'DISTANCE_ACCURACY_VALUE',
'Maximum model space distance between geometric entities at asserted c
onnectivities');
#7839=UNCERTAINTY_MEASURE_WITH_UNIT(LENGTH_MEASURE(0.001),#7898,
'DISTANCE_ACCURACY_VALUE',
'Maximum model space distance between geometric entities at asserted c
onnectivities');
#7840=UNCERTAINTY_MEASURE_WITH_UNIT(LENGTH_MEASURE(0.001),#7898,
'DISTANCE_ACCURACY_VALUE',
'Maximum model space distance between geometric entities at asserted c
onnectivities');
#7841=UNCERTAINTY_MEASURE_WITH_UNIT(LENGTH_MEASURE(0.001),#7898,
'DISTANCE_ACCURACY_VALUE',
'Maximum model space distance between geometric entities at asserted c
onnectivities');
#7842=UNCERTAINTY_MEASURE_WITH_UNIT(LENGTH_MEASURE(0.001),#7898,
'DISTANCE_ACCURACY_VALUE',
'Maximum model space distance between geometric entities at asserted c
onnectivities');
#7843=UNCERTAINTY_MEASURE_WITH_UNIT(LENGTH_MEASURE(0.001),#7898,
'DISTANCE_ACCURACY_VALUE',
'Maximum model space distance between geometric entities at asserted c
onnectivities');
#7844=UNCERTAINTY_MEASURE_WITH_UNIT(LENGTH_MEASURE(0.001),#7898,
'DISTANCE_ACCURACY_VALUE',
'Maximum model space distance between geometric entities at asserted c
onnectivities');
#7845=UNCERTAINTY_MEASURE_WITH_UNIT(LENGTH_MEASURE(0.001),#7898,
'DISTANCE_ACCURACY_VALUE',
'Maximum model space distance between geometric entities at asserted c
onnectivities');
#7846=UNCERTAINTY_MEASURE_WITH_UNIT(LENGTH_MEASURE(0.001),#7898,
'DISTANCE_ACCURACY_VALUE',
'Maximum model space distance between geometric entities at asserted c
onnectivities');
#7847=UNCERTAINTY_MEASURE_WITH_UNIT(LENGTH_MEASURE(0.001),#7898,
'DISTANCE_ACCURACY_VALUE',
'Maximum model space distance between geometric entities at asserted c
onnectivities');
#7848=UNCERTAINTY_MEASURE_WITH_UNIT(LENGTH_MEASURE(0.001),#7898,
'DISTANCE_ACCURACY_VALUE',
'Maximum model space distance between geometric entities at asserted c
onnectivities');
#7849=UNCERTAINTY_MEASURE_WITH_UNIT(LENGTH_MEASURE(0.001),#7898,
'DISTANCE_ACCURACY_VALUE',
'Maximum model space distance between geometric entities at asserted c
onnectivities');
#7850=UNCERTAINTY_MEASURE_WITH_UNIT(LENGTH_MEASURE(0.001),#7898,
'DISTANCE_ACCURACY_VALUE',
'Maximum model space distance between geometric entities at asserted c
onnectivities');
#7851=UNCERTAINTY_MEASURE_WITH_UNIT(LENGTH_MEASURE(0.001),#7898,
'DISTANCE_ACCURACY_VALUE',
'Maximum model space distance between geometric entities at asserted c
onnectivities');
#7852=UNCERTAINTY_MEASURE_WITH_UNIT(LENGTH_MEASURE(0.001),#7898,
'DISTANCE_ACCURACY_VALUE',
'Maximum model space distance between geometric entities at asserted c
onnectivities');
#7853=UNCERTAINTY_MEASURE_WITH_UNIT(LENGTH_MEASURE(0.001),#7898,
'DISTANCE_ACCURACY_VALUE',
'Maximum model space distance between geometric entities at asserted c
onnectivities');
#7854=UNCERTAINTY_MEASURE_WITH_UNIT(LENGTH_MEASURE(0.001),#7898,
'DISTANCE_ACCURACY_VALUE',
'Maximum model space distance between geometric entities at asserted c
onnectivities');
#7855=UNCERTAINTY_MEASURE_WITH_UNIT(LENGTH_MEASURE(0.001),#7898,
'DISTANCE_ACCURACY_VALUE',
'Maximum model space distance between geometric entities at asserted c
onnectivities');
#7856=UNCERTAINTY_MEASURE_WITH_UNIT(LENGTH_MEASURE(0.001),#7898,
'DISTANCE_ACCURACY_VALUE',
'Maximum model space distance between geometric entities at asserted c
onnectivities');
#7857=UNCERTAINTY_MEASURE_WITH_UNIT(LENGTH_MEASURE(0.001),#7898,
'DISTANCE_ACCURACY_VALUE',
'Maximum model space distance between geometric entities at asserted c
onnectivities');
#7858=UNCERTAINTY_MEASURE_WITH_UNIT(LENGTH_MEASURE(0.001),#7898,
'DISTANCE_ACCURACY_VALUE',
'Maximum model space distance between geometric entities at asserted c
onnectivities');
#7859=UNCERTAINTY_MEASURE_WITH_UNIT(LENGTH_MEASURE(0.001),#7898,
'DISTANCE_ACCURACY_VALUE',
'Maximum model space distance between geometric entities at asserted c
onnectivities');
#7860=UNCERTAINTY_MEASURE_WITH_UNIT(LENGTH_MEASURE(0.001),#7898,
'DISTANCE_ACCURACY_VALUE',
'Maximum model space distance between geometric entities at asserted c
onnectivities');
#7861=UNCERTAINTY_MEASURE_WITH_UNIT(LENGTH_MEASURE(0.001),#7898,
'DISTANCE_ACCURACY_VALUE',
'Maximum model space distance between geometric entities at asserted c
onnectivities');
#7862=UNCERTAINTY_MEASURE_WITH_UNIT(LENGTH_MEASURE(0.001),#7898,
'DISTANCE_ACCURACY_VALUE',
'Maximum model space distance between geometric entities at asserted c
onnectivities');
#7863=UNCERTAINTY_MEASURE_WITH_UNIT(LENGTH_MEASURE(0.001),#7898,
'DISTANCE_ACCURACY_VALUE',
'Maximum model space distance between geometric entities at asserted c
onnectivities');
#7864=UNCERTAINTY_MEASURE_WITH_UNIT(LENGTH_MEASURE(0.001),#7898,
'DISTANCE_ACCURACY_VALUE',
'Maximum model space distance between geometric entities at asserted c
onnectivities');
#7865=UNCERTAINTY_MEASURE_WITH_UNIT(LENGTH_MEASURE(0.001),#7898,
'DISTANCE_ACCURACY_VALUE',
'Maximum model space distance between geometric entities at asserted c
onnectivities');
#7866=(
GEOMETRIC_REPRESENTATION_CONTEXT(3)
GLOBAL_UNCERTAINTY_ASSIGNED_CONTEXT((#7834))
GLOBAL_UNIT_ASSIGNED_CONTEXT((#7898,#7900,#7901))
REPRESENTATION_CONTEXT('','3D')
);
#7867=(
GEOMETRIC_REPRESENTATION_CONTEXT(3)
GLOBAL_UNCERTAINTY_ASSIGNED_CONTEXT((#7835))
GLOBAL_UNIT_ASSIGNED_CONTEXT((#7898,#7900,#7901))
REPRESENTATION_CONTEXT('','3D')
);
#7868=(
GEOMETRIC_REPRESENTATION_CONTEXT(3)
GLOBAL_UNCERTAINTY_ASSIGNED_CONTEXT((#7836))
GLOBAL_UNIT_ASSIGNED_CONTEXT((#7898,#7900,#7901))
REPRESENTATION_CONTEXT('','3D')
);
#7869=(
GEOMETRIC_REPRESENTATION_CONTEXT(3)
GLOBAL_UNCERTAINTY_ASSIGNED_CONTEXT((#7837))
GLOBAL_UNIT_ASSIGNED_CONTEXT((#7898,#7900,#7901))
REPRESENTATION_CONTEXT('','3D')
);
#7870=(
GEOMETRIC_REPRESENTATION_CONTEXT(3)
GLOBAL_UNCERTAINTY_ASSIGNED_CONTEXT((#7838))
GLOBAL_UNIT_ASSIGNED_CONTEXT((#7898,#7900,#7901))
REPRESENTATION_CONTEXT('','3D')
);
#7871=(
GEOMETRIC_REPRESENTATION_CONTEXT(3)
GLOBAL_UNCERTAINTY_ASSIGNED_CONTEXT((#7839))
GLOBAL_UNIT_ASSIGNED_CONTEXT((#7898,#7900,#7901))
REPRESENTATION_CONTEXT('','3D')
);
#7872=(
GEOMETRIC_REPRESENTATION_CONTEXT(3)
GLOBAL_UNCERTAINTY_ASSIGNED_CONTEXT((#7840))
GLOBAL_UNIT_ASSIGNED_CONTEXT((#7898,#7900,#7901))
REPRESENTATION_CONTEXT('','3D')
);
#7873=(
GEOMETRIC_REPRESENTATION_CONTEXT(3)
GLOBAL_UNCERTAINTY_ASSIGNED_CONTEXT((#7841))
GLOBAL_UNIT_ASSIGNED_CONTEXT((#7898,#7900,#7901))
REPRESENTATION_CONTEXT('','3D')
);
#7874=(
GEOMETRIC_REPRESENTATION_CONTEXT(3)
GLOBAL_UNCERTAINTY_ASSIGNED_CONTEXT((#7842))
GLOBAL_UNIT_ASSIGNED_CONTEXT((#7898,#7900,#7901))
REPRESENTATION_CONTEXT('','3D')
);
#7875=(
GEOMETRIC_REPRESENTATION_CONTEXT(3)
GLOBAL_UNCERTAINTY_ASSIGNED_CONTEXT((#7843))
GLOBAL_UNIT_ASSIGNED_CONTEXT((#7898,#7900,#7901))
REPRESENTATION_CONTEXT('','3D')
);
#7876=(
GEOMETRIC_REPRESENTATION_CONTEXT(3)
GLOBAL_UNCERTAINTY_ASSIGNED_CONTEXT((#7844))
GLOBAL_UNIT_ASSIGNED_CONTEXT((#7898,#7900,#7901))
REPRESENTATION_CONTEXT('','3D')
);
#7877=(
GEOMETRIC_REPRESENTATION_CONTEXT(3)
GLOBAL_UNCERTAINTY_ASSIGNED_CONTEXT((#7845))
GLOBAL_UNIT_ASSIGNED_CONTEXT((#7898,#7900,#7901))
REPRESENTATION_CONTEXT('','3D')
);
#7878=(
GEOMETRIC_REPRESENTATION_CONTEXT(3)
GLOBAL_UNCERTAINTY_ASSIGNED_CONTEXT((#7846))
GLOBAL_UNIT_ASSIGNED_CONTEXT((#7898,#7900,#7901))
REPRESENTATION_CONTEXT('','3D')
);
#7879=(
GEOMETRIC_REPRESENTATION_CONTEXT(3)
GLOBAL_UNCERTAINTY_ASSIGNED_CONTEXT((#7847))
GLOBAL_UNIT_ASSIGNED_CONTEXT((#7898,#7900,#7901))
REPRESENTATION_CONTEXT('','3D')
);
#7880=(
GEOMETRIC_REPRESENTATION_CONTEXT(3)
GLOBAL_UNCERTAINTY_ASSIGNED_CONTEXT((#7848))
GLOBAL_UNIT_ASSIGNED_CONTEXT((#7898,#7900,#7901))
REPRESENTATION_CONTEXT('','3D')
);
#7881=(
GEOMETRIC_REPRESENTATION_CONTEXT(3)
GLOBAL_UNCERTAINTY_ASSIGNED_CONTEXT((#7849))
GLOBAL_UNIT_ASSIGNED_CONTEXT((#7898,#7900,#7901))
REPRESENTATION_CONTEXT('','3D')
);
#7882=(
GEOMETRIC_REPRESENTATION_CONTEXT(3)
GLOBAL_UNCERTAINTY_ASSIGNED_CONTEXT((#7850))
GLOBAL_UNIT_ASSIGNED_CONTEXT((#7898,#7900,#7901))
REPRESENTATION_CONTEXT('','3D')
);
#7883=(
GEOMETRIC_REPRESENTATION_CONTEXT(3)
GLOBAL_UNCERTAINTY_ASSIGNED_CONTEXT((#7851))
GLOBAL_UNIT_ASSIGNED_CONTEXT((#7898,#7900,#7901))
REPRESENTATION_CONTEXT('','3D')
);
#7884=(
GEOMETRIC_REPRESENTATION_CONTEXT(3)
GLOBAL_UNCERTAINTY_ASSIGNED_CONTEXT((#7852))
GLOBAL_UNIT_ASSIGNED_CONTEXT((#7898,#7900,#7901))
REPRESENTATION_CONTEXT('','3D')
);
#7885=(
GEOMETRIC_REPRESENTATION_CONTEXT(3)
GLOBAL_UNCERTAINTY_ASSIGNED_CONTEXT((#7853))
GLOBAL_UNIT_ASSIGNED_CONTEXT((#7898,#7900,#7901))
REPRESENTATION_CONTEXT('','3D')
);
#7886=(
GEOMETRIC_REPRESENTATION_CONTEXT(3)
GLOBAL_UNCERTAINTY_ASSIGNED_CONTEXT((#7854))
GLOBAL_UNIT_ASSIGNED_CONTEXT((#7898,#7900,#7901))
REPRESENTATION_CONTEXT('','3D')
);
#7887=(
GEOMETRIC_REPRESENTATION_CONTEXT(3)
GLOBAL_UNCERTAINTY_ASSIGNED_CONTEXT((#7855))
GLOBAL_UNIT_ASSIGNED_CONTEXT((#7898,#7900,#7901))
REPRESENTATION_CONTEXT('','3D')
);
#7888=(
GEOMETRIC_REPRESENTATION_CONTEXT(3)
GLOBAL_UNCERTAINTY_ASSIGNED_CONTEXT((#7856))
GLOBAL_UNIT_ASSIGNED_CONTEXT((#7898,#7900,#7901))
REPRESENTATION_CONTEXT('','3D')
);
#7889=(
GEOMETRIC_REPRESENTATION_CONTEXT(3)
GLOBAL_UNCERTAINTY_ASSIGNED_CONTEXT((#7857))
GLOBAL_UNIT_ASSIGNED_CONTEXT((#7898,#7900,#7901))
REPRESENTATION_CONTEXT('','3D')
);
#7890=(
GEOMETRIC_REPRESENTATION_CONTEXT(3)
GLOBAL_UNCERTAINTY_ASSIGNED_CONTEXT((#7858))
GLOBAL_UNIT_ASSIGNED_CONTEXT((#7898,#7900,#7901))
REPRESENTATION_CONTEXT('','3D')
);
#7891=(
GEOMETRIC_REPRESENTATION_CONTEXT(3)
GLOBAL_UNCERTAINTY_ASSIGNED_CONTEXT((#7859))
GLOBAL_UNIT_ASSIGNED_CONTEXT((#7898,#7900,#7901))
REPRESENTATION_CONTEXT('','3D')
);
#7892=(
GEOMETRIC_REPRESENTATION_CONTEXT(3)
GLOBAL_UNCERTAINTY_ASSIGNED_CONTEXT((#7860))
GLOBAL_UNIT_ASSIGNED_CONTEXT((#7898,#7900,#7901))
REPRESENTATION_CONTEXT('','3D')
);
#7893=(
GEOMETRIC_REPRESENTATION_CONTEXT(3)
GLOBAL_UNCERTAINTY_ASSIGNED_CONTEXT((#7861))
GLOBAL_UNIT_ASSIGNED_CONTEXT((#7898,#7900,#7901))
REPRESENTATION_CONTEXT('','3D')
);
#7894=(
GEOMETRIC_REPRESENTATION_CONTEXT(3)
GLOBAL_UNCERTAINTY_ASSIGNED_CONTEXT((#7862))
GLOBAL_UNIT_ASSIGNED_CONTEXT((#7898,#7900,#7901))
REPRESENTATION_CONTEXT('','3D')
);
#7895=(
GEOMETRIC_REPRESENTATION_CONTEXT(3)
GLOBAL_UNCERTAINTY_ASSIGNED_CONTEXT((#7863))
GLOBAL_UNIT_ASSIGNED_CONTEXT((#7898,#7900,#7901))
REPRESENTATION_CONTEXT('','3D')
);
#7896=(
GEOMETRIC_REPRESENTATION_CONTEXT(3)
GLOBAL_UNCERTAINTY_ASSIGNED_CONTEXT((#7864))
GLOBAL_UNIT_ASSIGNED_CONTEXT((#7898,#7900,#7901))
REPRESENTATION_CONTEXT('','3D')
);
#7897=(
GEOMETRIC_REPRESENTATION_CONTEXT(3)
GLOBAL_UNCERTAINTY_ASSIGNED_CONTEXT((#7865))
GLOBAL_UNIT_ASSIGNED_CONTEXT((#7898,#7900,#7901))
REPRESENTATION_CONTEXT('','3D')
);
#7898=(
LENGTH_UNIT()
NAMED_UNIT(*)
SI_UNIT(.CENTI.,.METRE.)
);
#7899=(
LENGTH_UNIT()
NAMED_UNIT(*)
SI_UNIT($,.METRE.)
);
#7900=(
NAMED_UNIT(*)
PLANE_ANGLE_UNIT()
SI_UNIT($,.RADIAN.)
);
#7901=(
NAMED_UNIT(*)
SI_UNIT($,.STERADIAN.)
SOLID_ANGLE_UNIT()
);
#7902=SHAPE_DEFINITION_REPRESENTATION(#7933,#7999);
#7903=SHAPE_DEFINITION_REPRESENTATION(#7934,#8000);
#7904=SHAPE_DEFINITION_REPRESENTATION(#7935,#8001);
#7905=SHAPE_DEFINITION_REPRESENTATION(#7936,#8002);
#7906=SHAPE_DEFINITION_REPRESENTATION(#7937,#8003);
#7907=SHAPE_DEFINITION_REPRESENTATION(#7938,#8004);
#7908=SHAPE_DEFINITION_REPRESENTATION(#7939,#8005);
#7909=SHAPE_DEFINITION_REPRESENTATION(#7940,#8006);
#7910=SHAPE_DEFINITION_REPRESENTATION(#7941,#8007);
#7911=SHAPE_DEFINITION_REPRESENTATION(#7942,#8008);
#7912=SHAPE_DEFINITION_REPRESENTATION(#7943,#8009);
#7913=SHAPE_DEFINITION_REPRESENTATION(#7944,#8010);
#7914=SHAPE_DEFINITION_REPRESENTATION(#7945,#8011);
#7915=SHAPE_DEFINITION_REPRESENTATION(#7946,#8012);
#7916=SHAPE_DEFINITION_REPRESENTATION(#7947,#8013);
#7917=SHAPE_DEFINITION_REPRESENTATION(#7948,#8014);
#7918=SHAPE_DEFINITION_REPRESENTATION(#7966,#8015);
#7919=SHAPE_DEFINITION_REPRESENTATION(#7967,#8016);
#7920=SHAPE_DEFINITION_REPRESENTATION(#7968,#8017);
#7921=SHAPE_DEFINITION_REPRESENTATION(#7969,#8018);
#7922=SHAPE_DEFINITION_REPRESENTATION(#7970,#8019);
#7923=SHAPE_DEFINITION_REPRESENTATION(#7971,#8020);
#7924=SHAPE_DEFINITION_REPRESENTATION(#7972,#8021);
#7925=SHAPE_DEFINITION_REPRESENTATION(#7973,#8022);
#7926=SHAPE_DEFINITION_REPRESENTATION(#7974,#8023);
#7927=SHAPE_DEFINITION_REPRESENTATION(#7975,#8024);
#7928=SHAPE_DEFINITION_REPRESENTATION(#7976,#8025);
#7929=SHAPE_DEFINITION_REPRESENTATION(#7977,#8026);
#7930=SHAPE_DEFINITION_REPRESENTATION(#7978,#8027);
#7931=SHAPE_DEFINITION_REPRESENTATION(#7979,#8028);
#7932=SHAPE_DEFINITION_REPRESENTATION(#7980,#8029);
#7933=PRODUCT_DEFINITION_SHAPE('',$,#8031);
#7934=PRODUCT_DEFINITION_SHAPE('',$,#8032);
#7935=PRODUCT_DEFINITION_SHAPE('',$,#8033);
#7936=PRODUCT_DEFINITION_SHAPE('',$,#8034);
#7937=PRODUCT_DEFINITION_SHAPE('',$,#8035);
#7938=PRODUCT_DEFINITION_SHAPE('',$,#8036);
#7939=PRODUCT_DEFINITION_SHAPE('',$,#8037);
#7940=PRODUCT_DEFINITION_SHAPE('',$,#8038);
#7941=PRODUCT_DEFINITION_SHAPE('',$,#8039);
#7942=PRODUCT_DEFINITION_SHAPE('',$,#8040);
#7943=PRODUCT_DEFINITION_SHAPE('',$,#8041);
#7944=PRODUCT_DEFINITION_SHAPE('',$,#8042);
#7945=PRODUCT_DEFINITION_SHAPE('',$,#8043);
#7946=PRODUCT_DEFINITION_SHAPE('',$,#8044);
#7947=PRODUCT_DEFINITION_SHAPE('',$,#8045);
#7948=PRODUCT_DEFINITION_SHAPE('',$,#8046);
#7949=PRODUCT_DEFINITION_SHAPE($,$,#116);
#7950=PRODUCT_DEFINITION_SHAPE($,$,#117);
#7951=PRODUCT_DEFINITION_SHAPE($,$,#118);
#7952=PRODUCT_DEFINITION_SHAPE($,$,#119);
#7953=PRODUCT_DEFINITION_SHAPE($,$,#120);
#7954=PRODUCT_DEFINITION_SHAPE($,$,#121);
#7955=PRODUCT_DEFINITION_SHAPE($,$,#122);
#7956=PRODUCT_DEFINITION_SHAPE($,$,#123);
#7957=PRODUCT_DEFINITION_SHAPE($,$,#124);
#7958=PRODUCT_DEFINITION_SHAPE($,$,#125);
#7959=PRODUCT_DEFINITION_SHAPE($,$,#126);
#7960=PRODUCT_DEFINITION_SHAPE($,$,#127);
#7961=PRODUCT_DEFINITION_SHAPE($,$,#128);
#7962=PRODUCT_DEFINITION_SHAPE($,$,#129);
#7963=PRODUCT_DEFINITION_SHAPE($,$,#130);
#7964=PRODUCT_DEFINITION_SHAPE($,$,#131);
#7965=PRODUCT_DEFINITION_SHAPE($,$,#132);
#7966=PRODUCT_DEFINITION_SHAPE('',$,#8047);
#7967=PRODUCT_DEFINITION_SHAPE('',$,#8048);
#7968=PRODUCT_DEFINITION_SHAPE('',$,#8049);
#7969=PRODUCT_DEFINITION_SHAPE('',$,#8050);
#7970=PRODUCT_DEFINITION_SHAPE('',$,#8051);
#7971=PRODUCT_DEFINITION_SHAPE('',$,#8052);
#7972=PRODUCT_DEFINITION_SHAPE('',$,#8053);
#7973=PRODUCT_DEFINITION_SHAPE('',$,#8054);
#7974=PRODUCT_DEFINITION_SHAPE('',$,#8055);
#7975=PRODUCT_DEFINITION_SHAPE('',$,#8056);
#7976=PRODUCT_DEFINITION_SHAPE('',$,#8057);
#7977=PRODUCT_DEFINITION_SHAPE('',$,#8058);
#7978=PRODUCT_DEFINITION_SHAPE('',$,#8059);
#7979=PRODUCT_DEFINITION_SHAPE('',$,#8060);
#7980=PRODUCT_DEFINITION_SHAPE('',$,#8061);
#7981=PRODUCT_DEFINITION_SHAPE($,$,#133);
#7982=PRODUCT_DEFINITION_SHAPE($,$,#134);
#7983=PRODUCT_DEFINITION_SHAPE($,$,#135);
#7984=PRODUCT_DEFINITION_SHAPE($,$,#136);
#7985=PRODUCT_DEFINITION_SHAPE($,$,#137);
#7986=PRODUCT_DEFINITION_SHAPE($,$,#138);
#7987=PRODUCT_DEFINITION_SHAPE($,$,#139);
#7988=PRODUCT_DEFINITION_SHAPE($,$,#140);
#7989=PRODUCT_DEFINITION_SHAPE($,$,#141);
#7990=PRODUCT_DEFINITION_SHAPE($,$,#142);
#7991=PRODUCT_DEFINITION_SHAPE($,$,#143);
#7992=PRODUCT_DEFINITION_SHAPE($,$,#144);
#7993=PRODUCT_DEFINITION_SHAPE($,$,#145);
#7994=PRODUCT_DEFINITION_SHAPE($,$,#146);
#7995=PRODUCT_DEFINITION_SHAPE($,$,#147);
#7996=PRODUCT_DEFINITION_SHAPE($,$,#148);
#7997=PRODUCT_DEFINITION_SHAPE($,$,#149);
#7998=PRODUCT_DEFINITION_SHAPE($,$,#150);
#7999=SHAPE_REPRESENTATION('',(#4589,#5068,#5069,#5070,#5071),#7866);
#8000=SHAPE_REPRESENTATION('',(#4590,#4884,#4885,#4886,#4887,#4888,#4889,
#4890,#4891,#4892,#4893,#4894,#4895,#4896,#4897,#4898,#4899,#4900),#7867);
#8001=SHAPE_REPRESENTATION('',(#4591),#7868);
#8002=SHAPE_REPRESENTATION('',(#4601),#7869);
#8003=SHAPE_REPRESENTATION('',(#4608),#7870);
#8004=SHAPE_REPRESENTATION('',(#4615),#7871);
#8005=SHAPE_REPRESENTATION('',(#4631),#7872);
#8006=SHAPE_REPRESENTATION('',(#4689),#7873);
#8007=SHAPE_REPRESENTATION('',(#4695),#7874);
#8008=SHAPE_REPRESENTATION('',(#4713),#7875);
#8009=SHAPE_REPRESENTATION('',(#4731),#7876);
#8010=SHAPE_REPRESENTATION('',(#4749),#7877);
#8011=SHAPE_REPRESENTATION('',(#4799),#7878);
#8012=SHAPE_REPRESENTATION('',(#4810),#7879);
#8013=SHAPE_REPRESENTATION('',(#4834),#7880);
#8014=SHAPE_REPRESENTATION('',(#4860),#7881);
#8015=SHAPE_REPRESENTATION('',(#4901,#5056,#5057,#5058,#5059),#7882);
#8016=SHAPE_REPRESENTATION('',(#4902),#7883);
#8017=SHAPE_REPRESENTATION('',(#4916),#7884);
#8018=SHAPE_REPRESENTATION('',(#4925),#7885);
#8019=SHAPE_REPRESENTATION('',(#4938,#5060,#5061,#5062,#5063),#7886);
#8020=SHAPE_REPRESENTATION('',(#4939),#7887);
#8021=SHAPE_REPRESENTATION('',(#4953),#7888);
#8022=SHAPE_REPRESENTATION('',(#4962),#7889);
#8023=SHAPE_REPRESENTATION('',(#4975,#5064,#5065,#5066,#5067),#7890);
#8024=SHAPE_REPRESENTATION('',(#4976),#7891);
#8025=SHAPE_REPRESENTATION('',(#4990),#7892);
#8026=SHAPE_REPRESENTATION('',(#4999),#7893);
#8027=SHAPE_REPRESENTATION('',(#5012,#5054,#5055),#7894);
#8028=SHAPE_REPRESENTATION('',(#5013),#7895);
#8029=SHAPE_REPRESENTATION('',(#5041),#7896);
#8030=PRODUCT_DEFINITION_CONTEXT('part definition',#8125,'design');
#8031=PRODUCT_DEFINITION('PAT-004','PAT-004',#8062,
#8030);
#8032=PRODUCT_DEFINITION('Column and manifold','Column and manifold',#8063,
#8030);
#8033=PRODUCT_DEFINITION('Base','Base',#8064,#8030);
#8034=PRODUCT_DEFINITION('Foot pad','Foot pad',#8065,#8030);
#8035=PRODUCT_DEFINITION('Foot pad (1)','Foot pad (1)',#8066,#8030);
#8036=PRODUCT_DEFINITION('Manifold shelf','Manifold shelf',#8067,#8030);
#8037=PRODUCT_DEFINITION('Manifold','Manifold',#8068,#8030);
#8038=PRODUCT_DEFINITION('Gallery closure','Gallery closure',#8069,#8030);
#8039=PRODUCT_DEFINITION('Ball clamp nut','Ball clamp nut',#8070,#8030);
#8040=PRODUCT_DEFINITION('Ball clamp nut (1)','Ball clamp nut (1)',#8071,
#8030);
#8041=PRODUCT_DEFINITION('Ball clamp nut (2)','Ball clamp nut (2)',#8072,
#8030);
#8042=PRODUCT_DEFINITION('Slotted Extrusion - 20 x 20 x 200 mm',
'Slotted Extrusion - 20 x 20 x 200 mm',#8073,#8030);
#8043=PRODUCT_DEFINITION('Flat Washer - M5','Flat Washer - M5',#8074,#8030);
#8044=PRODUCT_DEFINITION('M5x14 Cap Screw','M5x14 Cap Screw',#8075,#8030);
#8045=PRODUCT_DEFINITION('Cap Screw - M4x16','Cap Screw - M4x16',#8076,
#8030);
#8046=PRODUCT_DEFINITION(
'Hex Pipe Nipple - 1-4 Inch Tapered Pipe Thread',
'Hex Pipe Nipple - 1-4 Inch Tapered Pipe Thread',#8077,#8030);
#8047=PRODUCT_DEFINITION('Left nozzle','Left nozzle',#8078,#8030);
#8048=PRODUCT_DEFINITION('Nozzle ball','Nozzle ball',#8079,#8030);
#8049=PRODUCT_DEFINITION('Nozzle tube','Nozzle tube',#8080,#8030);
#8050=PRODUCT_DEFINITION('Nozzle tip','Nozzle tip',#8081,#8030);
#8051=PRODUCT_DEFINITION('Centre nozzle','Centre nozzle',#8082,#8030);
#8052=PRODUCT_DEFINITION('Nozzle ball (1)','Nozzle ball (1)',#8083,#8030);
#8053=PRODUCT_DEFINITION('Nozzle tube (1)','Nozzle tube (1)',#8084,#8030);
#8054=PRODUCT_DEFINITION('Nozzle tip (1)','Nozzle tip (1)',#8085,#8030);
#8055=PRODUCT_DEFINITION('Right nozzle','Right nozzle',#8086,#8030);
#8056=PRODUCT_DEFINITION('Nozzle ball (2)','Nozzle ball (2)',#8087,#8030);
#8057=PRODUCT_DEFINITION('Nozzle tube (2)','Nozzle tube (2)',#8088,#8030);
#8058=PRODUCT_DEFINITION('Nozzle tip (2)','Nozzle tip (2)',#8089,#8030);
#8059=PRODUCT_DEFINITION(
'Push-In Tube Fitting - 6 mm Tube, 1-8 Inch Tapered Pipe Thread',
'Push-In Tube Fitting - 6 mm Tube, 1-8 Inch Tapered Pipe Thread',#8090,
#8030);
#8060=PRODUCT_DEFINITION('Body','Body',#8091,#8030);
#8061=PRODUCT_DEFINITION('Release collar','Release collar',#8092,#8030);
#8062=PRODUCT_DEFINITION_FORMATION('',$,#8127);
#8063=PRODUCT_DEFINITION_FORMATION('',$,#8128);
#8064=PRODUCT_DEFINITION_FORMATION('',$,#8129);
#8065=PRODUCT_DEFINITION_FORMATION('',$,#8130);
#8066=PRODUCT_DEFINITION_FORMATION('',$,#8131);
#8067=PRODUCT_DEFINITION_FORMATION('',$,#8132);
#8068=PRODUCT_DEFINITION_FORMATION('',$,#8133);
#8069=PRODUCT_DEFINITION_FORMATION('',$,#8134);
#8070=PRODUCT_DEFINITION_FORMATION('',$,#8135);
#8071=PRODUCT_DEFINITION_FORMATION('',$,#8136);
#8072=PRODUCT_DEFINITION_FORMATION('',$,#8137);
#8073=PRODUCT_DEFINITION_FORMATION('',$,#8138);
#8074=PRODUCT_DEFINITION_FORMATION('',$,#8139);
#8075=PRODUCT_DEFINITION_FORMATION('',$,#8140);
#8076=PRODUCT_DEFINITION_FORMATION('',$,#8141);
#8077=PRODUCT_DEFINITION_FORMATION('',$,#8142);
#8078=PRODUCT_DEFINITION_FORMATION('',$,#8143);
#8079=PRODUCT_DEFINITION_FORMATION('',$,#8144);
#8080=PRODUCT_DEFINITION_FORMATION('',$,#8145);
#8081=PRODUCT_DEFINITION_FORMATION('',$,#8146);
#8082=PRODUCT_DEFINITION_FORMATION('',$,#8147);
#8083=PRODUCT_DEFINITION_FORMATION('',$,#8148);
#8084=PRODUCT_DEFINITION_FORMATION('',$,#8149);
#8085=PRODUCT_DEFINITION_FORMATION('',$,#8150);
#8086=PRODUCT_DEFINITION_FORMATION('',$,#8151);
#8087=PRODUCT_DEFINITION_FORMATION('',$,#8152);
#8088=PRODUCT_DEFINITION_FORMATION('',$,#8153);
#8089=PRODUCT_DEFINITION_FORMATION('',$,#8154);
#8090=PRODUCT_DEFINITION_FORMATION('',$,#8155);
#8091=PRODUCT_DEFINITION_FORMATION('',$,#8156);
#8092=PRODUCT_DEFINITION_FORMATION('',$,#8157);
#8093=PRODUCT_RELATED_PRODUCT_CATEGORY('PAT-004','PAT-004',(#8127));
#8094=PRODUCT_RELATED_PRODUCT_CATEGORY('Column and manifold',
'Column and manifold',(#8128));
#8095=PRODUCT_RELATED_PRODUCT_CATEGORY('Base','Base',(#8129));
#8096=PRODUCT_RELATED_PRODUCT_CATEGORY('Foot pad','Foot pad',(#8130));
#8097=PRODUCT_RELATED_PRODUCT_CATEGORY('Foot pad (1)','Foot pad (1)',(#8131));
#8098=PRODUCT_RELATED_PRODUCT_CATEGORY('Manifold shelf',
'Manifold shelf',(#8132));
#8099=PRODUCT_RELATED_PRODUCT_CATEGORY('Manifold','Manifold',(#8133));
#8100=PRODUCT_RELATED_PRODUCT_CATEGORY('Gallery closure',
'Gallery closure',(#8134));
#8101=PRODUCT_RELATED_PRODUCT_CATEGORY('Ball clamp nut',
'Ball clamp nut',(#8135));
#8102=PRODUCT_RELATED_PRODUCT_CATEGORY('Ball clamp nut (1)',
'Ball clamp nut (1)',(#8136));
#8103=PRODUCT_RELATED_PRODUCT_CATEGORY('Ball clamp nut (2)',
'Ball clamp nut (2)',(#8137));
#8104=PRODUCT_RELATED_PRODUCT_CATEGORY(
'Slotted Extrusion - 20 x 20 x 200 mm',
'Slotted Extrusion - 20 x 20 x 200 mm',(#8138));
#8105=PRODUCT_RELATED_PRODUCT_CATEGORY('Flat Washer - M5',
'Flat Washer - M5',(#8139));
#8106=PRODUCT_RELATED_PRODUCT_CATEGORY('M5x14 Cap Screw',
'M5x14 Cap Screw',(#8140));
#8107=PRODUCT_RELATED_PRODUCT_CATEGORY('Cap Screw - M4x16',
'Cap Screw - M4x16',(#8141));
#8108=PRODUCT_RELATED_PRODUCT_CATEGORY(
'Hex Pipe Nipple - 1-4 Inch Tapered Pipe Thread',
'Hex Pipe Nipple - 1-4 Inch Tapered Pipe Thread',(#8142));
#8109=PRODUCT_RELATED_PRODUCT_CATEGORY('Left nozzle','Left nozzle',(#8143));
#8110=PRODUCT_RELATED_PRODUCT_CATEGORY('Nozzle ball','Nozzle ball',(#8144));
#8111=PRODUCT_RELATED_PRODUCT_CATEGORY('Nozzle tube','Nozzle tube',(#8145));
#8112=PRODUCT_RELATED_PRODUCT_CATEGORY('Nozzle tip','Nozzle tip',(#8146));
#8113=PRODUCT_RELATED_PRODUCT_CATEGORY('Centre nozzle','Centre nozzle',
(#8147));
#8114=PRODUCT_RELATED_PRODUCT_CATEGORY('Nozzle ball (1)',
'Nozzle ball (1)',(#8148));
#8115=PRODUCT_RELATED_PRODUCT_CATEGORY('Nozzle tube (1)',
'Nozzle tube (1)',(#8149));
#8116=PRODUCT_RELATED_PRODUCT_CATEGORY('Nozzle tip (1)',
'Nozzle tip (1)',(#8150));
#8117=PRODUCT_RELATED_PRODUCT_CATEGORY('Right nozzle','Right nozzle',(#8151));
#8118=PRODUCT_RELATED_PRODUCT_CATEGORY('Nozzle ball (2)',
'Nozzle ball (2)',(#8152));
#8119=PRODUCT_RELATED_PRODUCT_CATEGORY('Nozzle tube (2)',
'Nozzle tube (2)',(#8153));
#8120=PRODUCT_RELATED_PRODUCT_CATEGORY('Nozzle tip (2)',
'Nozzle tip (2)',(#8154));
#8121=PRODUCT_RELATED_PRODUCT_CATEGORY(
'Push-In Tube Fitting - 6 mm Tube, 1-8 Inch Tapered Pipe Thread',
'Push-In Tube Fitting - 6 mm Tube, 1-8 Inch Tapered Pipe Thread',(#8155));
#8122=PRODUCT_RELATED_PRODUCT_CATEGORY('Body','Body',(#8156));
#8123=PRODUCT_RELATED_PRODUCT_CATEGORY('Release collar',
'Release collar',(#8157));
#8124=APPLICATION_PROTOCOL_DEFINITION('international standard',
'automotive_design',2009,#8125);
#8125=APPLICATION_CONTEXT(
'Core Data for Automotive Mechanical Design Process');
#8126=PRODUCT_CONTEXT('part definition',#8125,'mechanical');
#8127=PRODUCT('PAT-004','PAT-004',
'PAT-004',(#8126));
#8128=PRODUCT('Column and manifold','Column and manifold',
'Column and manifold',(#8126));
#8129=PRODUCT('Base','Base','Base',(#8126));
#8130=PRODUCT('Foot pad','Foot pad','Foot pad',(#8126));
#8131=PRODUCT('Foot pad (1)','Foot pad (1)','Foot pad (1)',(#8126));
#8132=PRODUCT('Manifold shelf','Manifold shelf','Manifold shelf',(#8126));
#8133=PRODUCT('Manifold','Manifold','Manifold',(#8126));
#8134=PRODUCT('Gallery closure','Gallery closure','Gallery closure',(#8126));
#8135=PRODUCT('Ball clamp nut','Ball clamp nut','Ball clamp nut',(#8126));
#8136=PRODUCT('Ball clamp nut (1)','Ball clamp nut (1)','Ball clamp nut (1)',
(#8126));
#8137=PRODUCT('Ball clamp nut (2)','Ball clamp nut (2)','Ball clamp nut (2)',
(#8126));
#8138=PRODUCT('Slotted Extrusion - 20 x 20 x 200 mm',
'Slotted Extrusion - 20 x 20 x 200 mm',
'Slotted Extrusion - 20 x 20 x 200 mm',(#8126));
#8139=PRODUCT('Flat Washer - M5','Flat Washer - M5','Flat Washer - M5',
(#8126));
#8140=PRODUCT('M5x14 Cap Screw','M5x14 Cap Screw','M5x14 Cap Screw',(#8126));
#8141=PRODUCT('Cap Screw - M4x16','Cap Screw - M4x16',
'Cap Screw - M4x16',(#8126));
#8142=PRODUCT('Hex Pipe Nipple - 1-4 Inch Tapered Pipe Thread',
'Hex Pipe Nipple - 1-4 Inch Tapered Pipe Thread',
'Hex Pipe Nipple - 1-4 Inch Tapered Pipe Thread',(#8126));
#8143=PRODUCT('Left nozzle','Left nozzle','Left nozzle',(#8126));
#8144=PRODUCT('Nozzle ball','Nozzle ball','Nozzle ball',(#8126));
#8145=PRODUCT('Nozzle tube','Nozzle tube','Nozzle tube',(#8126));
#8146=PRODUCT('Nozzle tip','Nozzle tip','Nozzle tip',(#8126));
#8147=PRODUCT('Centre nozzle','Centre nozzle','Centre nozzle',(#8126));
#8148=PRODUCT('Nozzle ball (1)','Nozzle ball (1)','Nozzle ball (1)',(#8126));
#8149=PRODUCT('Nozzle tube (1)','Nozzle tube (1)','Nozzle tube (1)',(#8126));
#8150=PRODUCT('Nozzle tip (1)','Nozzle tip (1)','Nozzle tip (1)',(#8126));
#8151=PRODUCT('Right nozzle','Right nozzle','Right nozzle',(#8126));
#8152=PRODUCT('Nozzle ball (2)','Nozzle ball (2)','Nozzle ball (2)',(#8126));
#8153=PRODUCT('Nozzle tube (2)','Nozzle tube (2)','Nozzle tube (2)',(#8126));
#8154=PRODUCT('Nozzle tip (2)','Nozzle tip (2)','Nozzle tip (2)',(#8126));
#8155=PRODUCT(
'Push-In Tube Fitting - 6 mm Tube, 1-8 Inch Tapered Pipe Thread',
'Push-In Tube Fitting - 6 mm Tube, 1-8 Inch Tapered Pipe Thread',
'Push-In Tube Fitting - 6 mm Tube, 1-8 Inch Tapered Pipe Thread',(#8126));
#8156=PRODUCT('Body','Body','Body',(#8126));
#8157=PRODUCT('Release collar','Release collar','Release collar',(#8126));
#8158=PRESENTATION_STYLE_ASSIGNMENT((#8163));
#8159=PRESENTATION_STYLE_ASSIGNMENT((#8164));
#8160=PRESENTATION_STYLE_ASSIGNMENT((#8165));
#8161=PRESENTATION_STYLE_ASSIGNMENT((#8166));
#8162=PRESENTATION_STYLE_ASSIGNMENT((#8167));
#8163=SURFACE_STYLE_USAGE(.BOTH.,#8168);
#8164=SURFACE_STYLE_USAGE(.BOTH.,#8169);
#8165=SURFACE_STYLE_USAGE(.BOTH.,#8170);
#8166=SURFACE_STYLE_USAGE(.BOTH.,#8171);
#8167=SURFACE_STYLE_USAGE(.BOTH.,#8172);
#8168=SURFACE_SIDE_STYLE('',(#8173));
#8169=SURFACE_SIDE_STYLE('',(#8174));
#8170=SURFACE_SIDE_STYLE('',(#8175));
#8171=SURFACE_SIDE_STYLE('',(#8176));
#8172=SURFACE_SIDE_STYLE('',(#8177));
#8173=SURFACE_STYLE_FILL_AREA(#8178);
#8174=SURFACE_STYLE_FILL_AREA(#8179);
#8175=SURFACE_STYLE_FILL_AREA(#8180);
#8176=SURFACE_STYLE_FILL_AREA(#8181);
#8177=SURFACE_STYLE_FILL_AREA(#8182);
#8178=FILL_AREA_STYLE('Steel - Satin',(#8183));
#8179=FILL_AREA_STYLE('CAD Library Painted - Deep blue',(#8184));
#8180=FILL_AREA_STYLE('CAD Library Painted - Graphite',(#8185));
#8181=FILL_AREA_STYLE('CAD Library Painted - Engineering blue',(#8186));
#8182=FILL_AREA_STYLE('CAD Library Painted - Steel gray',(#8187));
#8183=FILL_AREA_STYLE_COLOUR('Steel - Satin',#8188);
#8184=FILL_AREA_STYLE_COLOUR('CAD Library Painted - Deep blue',#8189);
#8185=FILL_AREA_STYLE_COLOUR('CAD Library Painted - Graphite',#8190);
#8186=FILL_AREA_STYLE_COLOUR('CAD Library Painted - Engineering blue',#8191);
#8187=FILL_AREA_STYLE_COLOUR('CAD Library Painted - Steel gray',#8192);
#8188=COLOUR_RGB('Steel - Satin',0.627450980392157,0.627450980392157,0.627450980392157);
#8189=COLOUR_RGB('CAD Library Painted - Deep blue',0.0784313725490196,0.203921568627451,
0.349019607843137);
#8190=COLOUR_RGB('CAD Library Painted - Graphite',0.168627450980392,0.192156862745098,
0.231372549019608);
#8191=COLOUR_RGB('CAD Library Painted - Engineering blue',0.12156862745098,
0.356862745098039,0.6);
#8192=COLOUR_RGB('CAD Library Painted - Steel gray',0.592156862745098,0.631372549019608,
0.67843137254902);
#8193=COLOUR_RGB('Dark Blue',0.08,0.2,0.34);
#8194=FILL_AREA_STYLE_COLOUR('',#8193);
#8195=FILL_AREA_STYLE('',(#8194));
#8196=SURFACE_STYLE_FILL_AREA(#8195);
#8197=SURFACE_SIDE_STYLE('',(#8196));
#8198=SURFACE_STYLE_USAGE(.BOTH.,#8197);
#8199=PRESENTATION_STYLE_ASSIGNMENT((#8198));
#8200=COLOUR_RGB('Light Blue',0.38,0.62,0.78);
#8201=FILL_AREA_STYLE_COLOUR('',#8200);
#8202=FILL_AREA_STYLE('',(#8201));
#8203=SURFACE_STYLE_FILL_AREA(#8202);
#8204=SURFACE_SIDE_STYLE('',(#8203));
#8205=SURFACE_STYLE_USAGE(.BOTH.,#8204);
#8206=PRESENTATION_STYLE_ASSIGNMENT((#8205));
#8207=COLOUR_RGB('Sky Blue',0.24,0.69,0.87);
#8208=FILL_AREA_STYLE_COLOUR('',#8207);
#8209=FILL_AREA_STYLE('',(#8208));
#8210=SURFACE_STYLE_FILL_AREA(#8209);
#8211=SURFACE_SIDE_STYLE('',(#8210));
#8212=SURFACE_STYLE_USAGE(.BOTH.,#8211);
#8213=PRESENTATION_STYLE_ASSIGNMENT((#8212));
#8214=COLOUR_RGB('Grey',0.48,0.52,0.57);
#8215=FILL_AREA_STYLE_COLOUR('',#8214);
#8216=FILL_AREA_STYLE('',(#8215));
#8217=SURFACE_STYLE_FILL_AREA(#8216);
#8218=SURFACE_SIDE_STYLE('',(#8217));
#8219=SURFACE_STYLE_USAGE(.BOTH.,#8218);
#8220=PRESENTATION_STYLE_ASSIGNMENT((#8219));
#8221=COLOUR_RGB('Black',0.12,0.14,0.17);
#8222=FILL_AREA_STYLE_COLOUR('',#8221);
#8223=FILL_AREA_STYLE('',(#8222));
#8224=SURFACE_STYLE_FILL_AREA(#8223);
#8225=SURFACE_SIDE_STYLE('',(#8224));
#8226=SURFACE_STYLE_USAGE(.BOTH.,#8225);
#8227=PRESENTATION_STYLE_ASSIGNMENT((#8226));
#8228=COLOUR_RGB('Off White',0.89,0.88,0.83);
#8229=FILL_AREA_STYLE_COLOUR('',#8228);
#8230=FILL_AREA_STYLE('',(#8229));
#8231=SURFACE_STYLE_FILL_AREA(#8230);
#8232=SURFACE_SIDE_STYLE('',(#8231));
#8233=SURFACE_STYLE_USAGE(.BOTH.,#8232);
#8234=PRESENTATION_STYLE_ASSIGNMENT((#8233));
ENDSEC;
END-ISO-10303-21;
